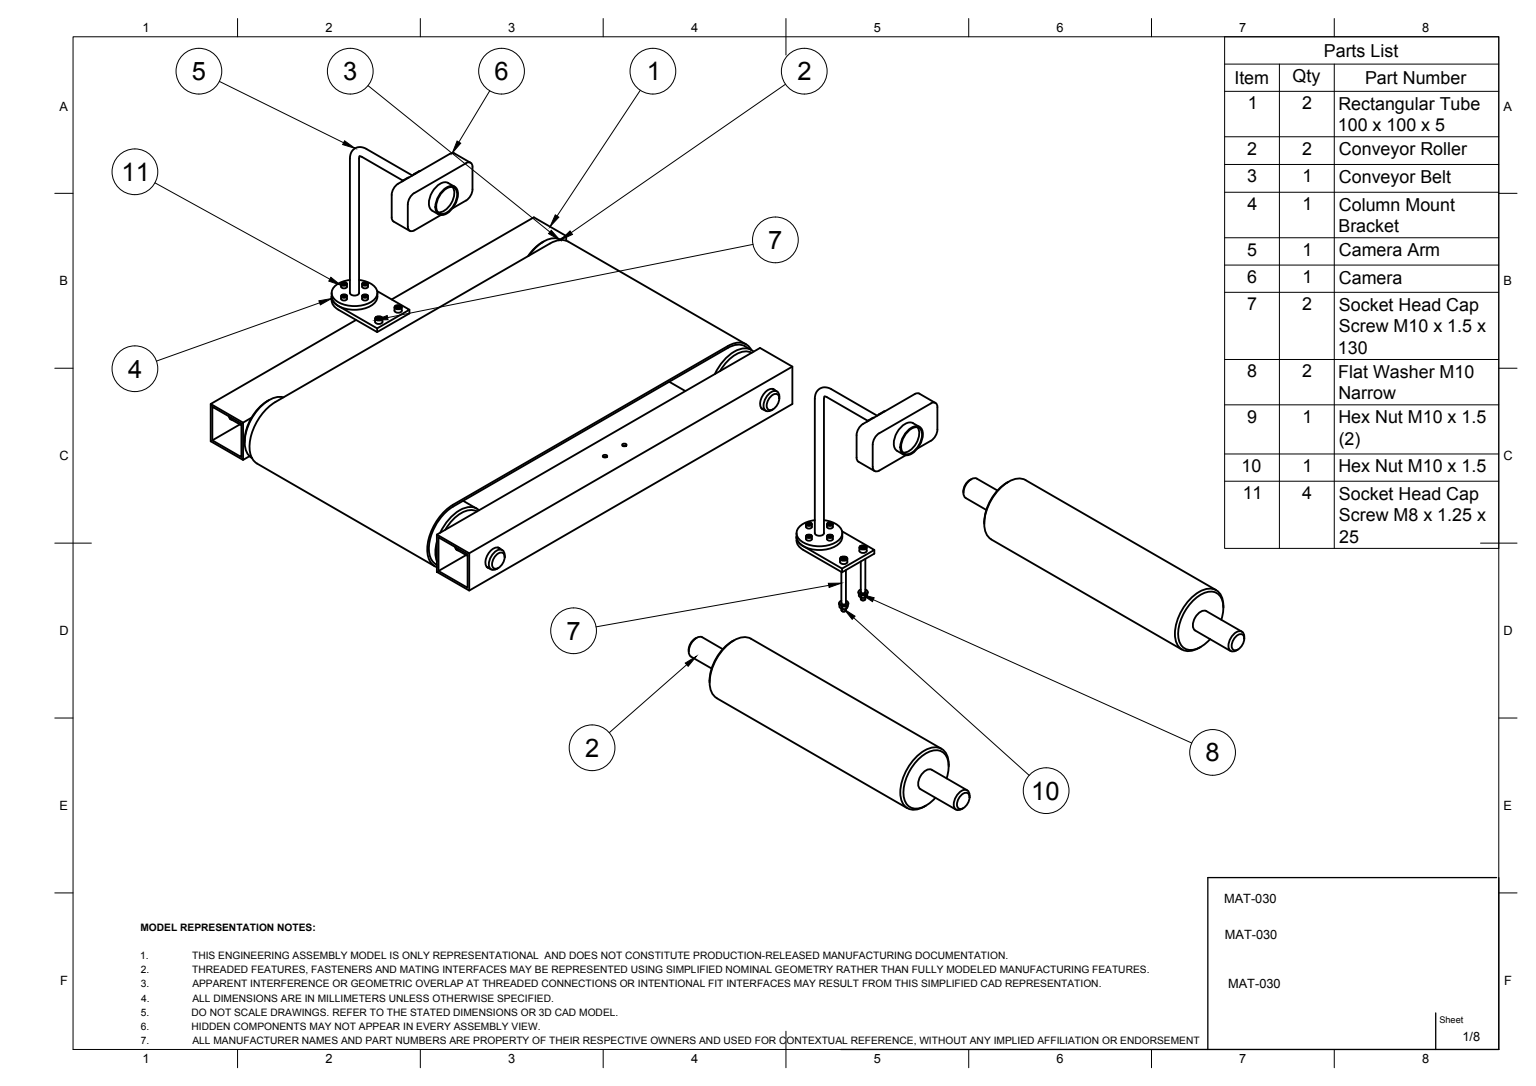
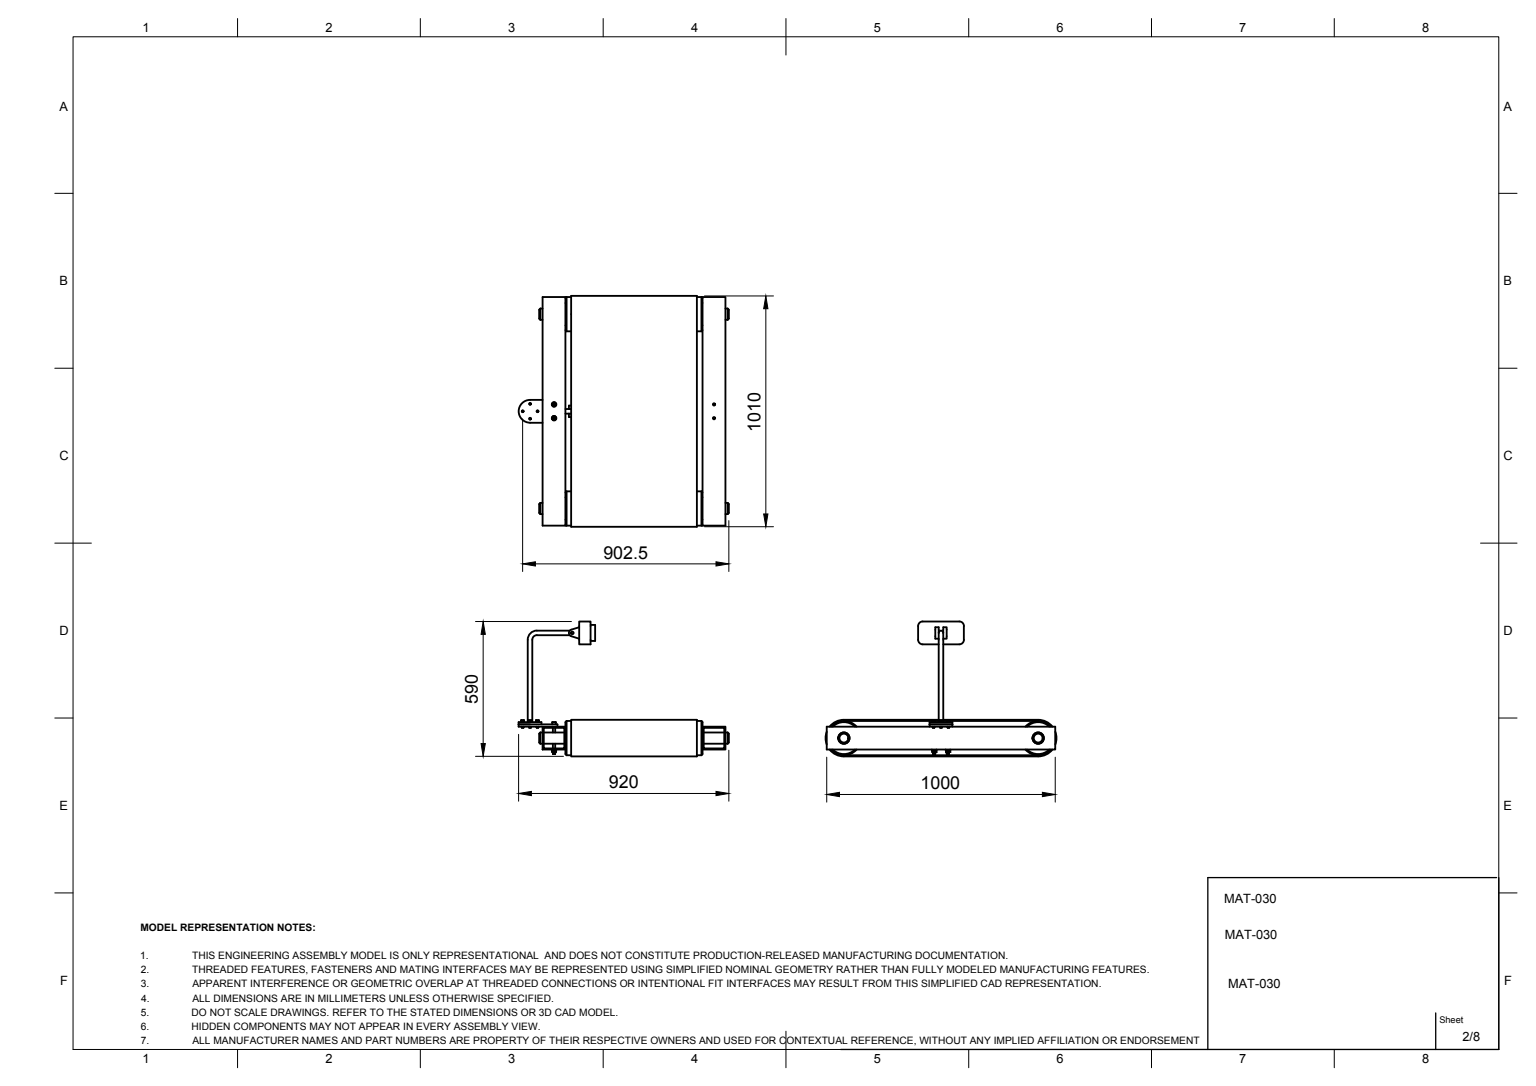
ISO-10303-21;
HEADER;
/* Generated by software containing ST-Developer
 * from STEP Tools, Inc. (www.steptools.com) 
 */

FILE_DESCRIPTION(
/* description */ ('STEP AP214'),
/* implementation_level */ '2;1');

FILE_NAME(
/* name */ 'MAT-030.step',
/* time_stamp */ '2026-11-14T06:43:04-08:00',
/* author */ (''),
/* organization */ (''),
/* preprocessor_version */ 'ST-DEVELOPER v20.2',
/* originating_system */ 'Autodesk Translation Framework v15.17.0.0',
/* authorisation */ '');

FILE_SCHEMA (('AUTOMOTIVE_DESIGN { 1 0 10303 214 3 1 1 }'));
ENDSEC;

DATA;
#10=MECHANICAL_DESIGN_GEOMETRIC_PRESENTATION_REPRESENTATION('',(#198,#199,
#200,#201,#202,#203,#204,#205,#206,#207,#208),#5658);
#11=ITEM_DEFINED_TRANSFORMATION($,$,#3397,#3541);
#12=ITEM_DEFINED_TRANSFORMATION($,$,#3432,#3542);
#13=ITEM_DEFINED_TRANSFORMATION($,$,#3194,#3543);
#14=ITEM_DEFINED_TRANSFORMATION($,$,#3213,#3544);
#15=ITEM_DEFINED_TRANSFORMATION($,$,#3240,#3545);
#16=ITEM_DEFINED_TRANSFORMATION($,$,#3278,#3546);
#17=ITEM_DEFINED_TRANSFORMATION($,$,#3456,#3547);
#18=ITEM_DEFINED_TRANSFORMATION($,$,#3494,#3548);
#19=ITEM_DEFINED_TRANSFORMATION($,$,#3325,#3549);
#20=ITEM_DEFINED_TRANSFORMATION($,$,#3361,#3550);
#21=ITEM_DEFINED_TRANSFORMATION($,$,#3503,#3551);
#22=ITEM_DEFINED_TRANSFORMATION($,$,#3397,#3552);
#23=ITEM_DEFINED_TRANSFORMATION($,$,#3432,#3553);
#24=ITEM_DEFINED_TRANSFORMATION($,$,#3456,#3554);
#25=ITEM_DEFINED_TRANSFORMATION($,$,#3494,#3555);
#26=ITEM_DEFINED_TRANSFORMATION($,$,#3503,#3556);
#27=ITEM_DEFINED_TRANSFORMATION($,$,#3503,#3557);
#28=ITEM_DEFINED_TRANSFORMATION($,$,#3503,#3558);
#29=(
REPRESENTATION_RELATIONSHIP($,$,#5712,#5705)
REPRESENTATION_RELATIONSHIP_WITH_TRANSFORMATION(#11)
SHAPE_REPRESENTATION_RELATIONSHIP()
);
#30=(
REPRESENTATION_RELATIONSHIP($,$,#5713,#5705)
REPRESENTATION_RELATIONSHIP_WITH_TRANSFORMATION(#12)
SHAPE_REPRESENTATION_RELATIONSHIP()
);
#31=(
REPRESENTATION_RELATIONSHIP($,$,#5706,#5705)
REPRESENTATION_RELATIONSHIP_WITH_TRANSFORMATION(#13)
SHAPE_REPRESENTATION_RELATIONSHIP()
);
#32=(
REPRESENTATION_RELATIONSHIP($,$,#5707,#5705)
REPRESENTATION_RELATIONSHIP_WITH_TRANSFORMATION(#14)
SHAPE_REPRESENTATION_RELATIONSHIP()
);
#33=(
REPRESENTATION_RELATIONSHIP($,$,#5708,#5705)
REPRESENTATION_RELATIONSHIP_WITH_TRANSFORMATION(#15)
SHAPE_REPRESENTATION_RELATIONSHIP()
);
#34=(
REPRESENTATION_RELATIONSHIP($,$,#5709,#5705)
REPRESENTATION_RELATIONSHIP_WITH_TRANSFORMATION(#16)
SHAPE_REPRESENTATION_RELATIONSHIP()
);
#35=(
REPRESENTATION_RELATIONSHIP($,$,#5714,#5705)
REPRESENTATION_RELATIONSHIP_WITH_TRANSFORMATION(#17)
SHAPE_REPRESENTATION_RELATIONSHIP()
);
#36=(
REPRESENTATION_RELATIONSHIP($,$,#5715,#5705)
REPRESENTATION_RELATIONSHIP_WITH_TRANSFORMATION(#18)
SHAPE_REPRESENTATION_RELATIONSHIP()
);
#37=(
REPRESENTATION_RELATIONSHIP($,$,#5710,#5705)
REPRESENTATION_RELATIONSHIP_WITH_TRANSFORMATION(#19)
SHAPE_REPRESENTATION_RELATIONSHIP()
);
#38=(
REPRESENTATION_RELATIONSHIP($,$,#5711,#5705)
REPRESENTATION_RELATIONSHIP_WITH_TRANSFORMATION(#20)
SHAPE_REPRESENTATION_RELATIONSHIP()
);
#39=(
REPRESENTATION_RELATIONSHIP($,$,#5716,#5705)
REPRESENTATION_RELATIONSHIP_WITH_TRANSFORMATION(#21)
SHAPE_REPRESENTATION_RELATIONSHIP()
);
#40=(
REPRESENTATION_RELATIONSHIP($,$,#5712,#5705)
REPRESENTATION_RELATIONSHIP_WITH_TRANSFORMATION(#22)
SHAPE_REPRESENTATION_RELATIONSHIP()
);
#41=(
REPRESENTATION_RELATIONSHIP($,$,#5713,#5705)
REPRESENTATION_RELATIONSHIP_WITH_TRANSFORMATION(#23)
SHAPE_REPRESENTATION_RELATIONSHIP()
);
#42=(
REPRESENTATION_RELATIONSHIP($,$,#5714,#5705)
REPRESENTATION_RELATIONSHIP_WITH_TRANSFORMATION(#24)
SHAPE_REPRESENTATION_RELATIONSHIP()
);
#43=(
REPRESENTATION_RELATIONSHIP($,$,#5715,#5705)
REPRESENTATION_RELATIONSHIP_WITH_TRANSFORMATION(#25)
SHAPE_REPRESENTATION_RELATIONSHIP()
);
#44=(
REPRESENTATION_RELATIONSHIP($,$,#5716,#5705)
REPRESENTATION_RELATIONSHIP_WITH_TRANSFORMATION(#26)
SHAPE_REPRESENTATION_RELATIONSHIP()
);
#45=(
REPRESENTATION_RELATIONSHIP($,$,#5716,#5705)
REPRESENTATION_RELATIONSHIP_WITH_TRANSFORMATION(#27)
SHAPE_REPRESENTATION_RELATIONSHIP()
);
#46=(
REPRESENTATION_RELATIONSHIP($,$,#5716,#5705)
REPRESENTATION_RELATIONSHIP_WITH_TRANSFORMATION(#28)
SHAPE_REPRESENTATION_RELATIONSHIP()
);
#47=CONTEXT_DEPENDENT_SHAPE_REPRESENTATION(#29,#5687);
#48=CONTEXT_DEPENDENT_SHAPE_REPRESENTATION(#30,#5688);
#49=CONTEXT_DEPENDENT_SHAPE_REPRESENTATION(#31,#5689);
#50=CONTEXT_DEPENDENT_SHAPE_REPRESENTATION(#32,#5690);
#51=CONTEXT_DEPENDENT_SHAPE_REPRESENTATION(#33,#5691);
#52=CONTEXT_DEPENDENT_SHAPE_REPRESENTATION(#34,#5692);
#53=CONTEXT_DEPENDENT_SHAPE_REPRESENTATION(#35,#5693);
#54=CONTEXT_DEPENDENT_SHAPE_REPRESENTATION(#36,#5694);
#55=CONTEXT_DEPENDENT_SHAPE_REPRESENTATION(#37,#5695);
#56=CONTEXT_DEPENDENT_SHAPE_REPRESENTATION(#38,#5696);
#57=CONTEXT_DEPENDENT_SHAPE_REPRESENTATION(#39,#5697);
#58=CONTEXT_DEPENDENT_SHAPE_REPRESENTATION(#40,#5698);
#59=CONTEXT_DEPENDENT_SHAPE_REPRESENTATION(#41,#5699);
#60=CONTEXT_DEPENDENT_SHAPE_REPRESENTATION(#42,#5700);
#61=CONTEXT_DEPENDENT_SHAPE_REPRESENTATION(#43,#5701);
#62=CONTEXT_DEPENDENT_SHAPE_REPRESENTATION(#44,#5702);
#63=CONTEXT_DEPENDENT_SHAPE_REPRESENTATION(#45,#5703);
#64=CONTEXT_DEPENDENT_SHAPE_REPRESENTATION(#46,#5704);
#65=NEXT_ASSEMBLY_USAGE_OCCURRENCE('Rectangular Tube 100 x 100 x 5:1',
'Rectangular Tube 100 x 100 x 5:1','Rectangular Tube 100 x 100 x 5:1',#5718,
#5725,'Rectangular Tube 100 x 100 x 5:1');
#66=NEXT_ASSEMBLY_USAGE_OCCURRENCE('Conveyor Roller:1',
'Conveyor Roller:1','Conveyor Roller:1',#5718,#5726,'Conveyor Roller:1');
#67=NEXT_ASSEMBLY_USAGE_OCCURRENCE('Conveyor Belt:1','Conveyor Belt:1',
'Conveyor Belt:1',#5718,#5719,'Conveyor Belt:1');
#68=NEXT_ASSEMBLY_USAGE_OCCURRENCE('Column Mount Bracket:1',
'Column Mount Bracket:1','Column Mount Bracket:1',#5718,#5720,
'Column Mount Bracket:1');
#69=NEXT_ASSEMBLY_USAGE_OCCURRENCE('Camera Arm:1','Camera Arm:1',
'Camera Arm:1',#5718,#5721,'Camera Arm:1');
#70=NEXT_ASSEMBLY_USAGE_OCCURRENCE('Camera:1','Camera:1','Camera:1',#5718,
#5722,'Camera:1');
#71=NEXT_ASSEMBLY_USAGE_OCCURRENCE(
'Socket Head Cap Screw M10 x 1.5 x 130:1',
'Socket Head Cap Screw M10 x 1.5 x 130:1',
'Socket Head Cap Screw M10 x 1.5 x 130:1',#5718,#5727,
'Socket Head Cap Screw M10 x 1.5 x 130:1');
#72=NEXT_ASSEMBLY_USAGE_OCCURRENCE('Flat Washer M10 Narrow:1',
'Flat Washer M10 Narrow:1','Flat Washer M10 Narrow:1',#5718,#5728,
'Flat Washer M10 Narrow:1');
#73=NEXT_ASSEMBLY_USAGE_OCCURRENCE('Hex Nut M10 x 1.5 (2):1',
'Hex Nut M10 x 1.5 (2):1','Hex Nut M10 x 1.5 (2):1',#5718,#5723,
'Hex Nut M10 x 1.5 (2):1');
#74=NEXT_ASSEMBLY_USAGE_OCCURRENCE('Hex Nut M10 x 1.5:1',
'Hex Nut M10 x 1.5:1','Hex Nut M10 x 1.5:1',#5718,#5724,
'Hex Nut M10 x 1.5:1');
#75=NEXT_ASSEMBLY_USAGE_OCCURRENCE(
'Socket Head Cap Screw M8 x 1.25 x 25:1',
'Socket Head Cap Screw M8 x 1.25 x 25:1',
'Socket Head Cap Screw M8 x 1.25 x 25:1',#5718,#5729,
'Socket Head Cap Screw M8 x 1.25 x 25:1');
#76=NEXT_ASSEMBLY_USAGE_OCCURRENCE('Rectangular Tube 100 x 100 x 5:2',
'Rectangular Tube 100 x 100 x 5:2','Rectangular Tube 100 x 100 x 5:2',#5718,
#5725,'Rectangular Tube 100 x 100 x 5:2');
#77=NEXT_ASSEMBLY_USAGE_OCCURRENCE('Conveyor Roller:2',
'Conveyor Roller:2','Conveyor Roller:2',#5718,#5726,'Conveyor Roller:2');
#78=NEXT_ASSEMBLY_USAGE_OCCURRENCE(
'Socket Head Cap Screw M10 x 1.5 x 130:2',
'Socket Head Cap Screw M10 x 1.5 x 130:2',
'Socket Head Cap Screw M10 x 1.5 x 130:2',#5718,#5727,
'Socket Head Cap Screw M10 x 1.5 x 130:2');
#79=NEXT_ASSEMBLY_USAGE_OCCURRENCE('Flat Washer M10 Narrow:2',
'Flat Washer M10 Narrow:2','Flat Washer M10 Narrow:2',#5718,#5728,
'Flat Washer M10 Narrow:2');
#80=NEXT_ASSEMBLY_USAGE_OCCURRENCE(
'Socket Head Cap Screw M8 x 1.25 x 25:2',
'Socket Head Cap Screw M8 x 1.25 x 25:2',
'Socket Head Cap Screw M8 x 1.25 x 25:2',#5718,#5729,
'Socket Head Cap Screw M8 x 1.25 x 25:2');
#81=NEXT_ASSEMBLY_USAGE_OCCURRENCE(
'Socket Head Cap Screw M8 x 1.25 x 25:3',
'Socket Head Cap Screw M8 x 1.25 x 25:3',
'Socket Head Cap Screw M8 x 1.25 x 25:3',#5718,#5729,
'Socket Head Cap Screw M8 x 1.25 x 25:3');
#82=NEXT_ASSEMBLY_USAGE_OCCURRENCE(
'Socket Head Cap Screw M8 x 1.25 x 25:4',
'Socket Head Cap Screw M8 x 1.25 x 25:4',
'Socket Head Cap Screw M8 x 1.25 x 25:4',#5718,#5729,
'Socket Head Cap Screw M8 x 1.25 x 25:4');
#83=CONICAL_SURFACE('',#3349,8.,1.0471975511966);
#84=CONICAL_SURFACE('',#3350,8.,1.0471975511966);
#85=CONICAL_SURFACE('',#3351,8.,1.0471975511966);
#86=CONICAL_SURFACE('',#3352,8.,1.0471975511966);
#87=CONICAL_SURFACE('',#3353,8.,1.0471975511966);
#88=CONICAL_SURFACE('',#3354,8.,1.0471975511966);
#89=CONICAL_SURFACE('',#3355,8.,1.0471975511966);
#90=CONICAL_SURFACE('',#3356,8.,1.0471975511966);
#91=CONICAL_SURFACE('',#3357,8.,1.0471975511966);
#92=CONICAL_SURFACE('',#3358,8.,1.0471975511966);
#93=CONICAL_SURFACE('',#3359,8.,1.0471975511966);
#94=CONICAL_SURFACE('',#3360,8.,1.0471975511966);
#95=CONICAL_SURFACE('',#3385,8.,1.0471975511966);
#96=CONICAL_SURFACE('',#3386,8.,1.0471975511966);
#97=CONICAL_SURFACE('',#3387,8.,1.0471975511966);
#98=CONICAL_SURFACE('',#3388,8.,1.0471975511966);
#99=CONICAL_SURFACE('',#3389,8.,1.0471975511966);
#100=CONICAL_SURFACE('',#3390,8.,1.0471975511966);
#101=CONICAL_SURFACE('',#3391,8.,1.0471975511966);
#102=CONICAL_SURFACE('',#3392,8.,1.0471975511966);
#103=CONICAL_SURFACE('',#3393,8.,1.0471975511966);
#104=CONICAL_SURFACE('',#3394,8.,1.0471975511966);
#105=CONICAL_SURFACE('',#3395,8.,1.0471975511966);
#106=CONICAL_SURFACE('',#3396,8.,1.0471975511966);
#107=CONICAL_SURFACE('',#3433,70.0000000000001,0.785398163397444);
#108=CONICAL_SURFACE('',#3437,19.5,0.785398163397451);
#109=CONICAL_SURFACE('',#3441,24.5,0.78539816339745);
#110=CONICAL_SURFACE('',#3444,75.,0.785398163397444);
#111=CONICAL_SURFACE('',#3457,4.0575,1.04719755119659);
#112=CONICAL_SURFACE('',#3469,7.,0.785398163397448);
#113=CONICAL_SURFACE('',#3477,4.172,0.785398163397561);
#114=CONICAL_SURFACE('',#3504,3.0475,1.04719755119659);
#115=CONICAL_SURFACE('',#3516,3.3095,0.785398163397565);
#116=CONICAL_SURFACE('',#3524,5.7,0.785398163397447);
#117=(
BOUNDED_CURVE()
B_SPLINE_CURVE(2,(#4998,#4999,#5000),.UNSPECIFIED.,.F.,.F.)
B_SPLINE_CURVE_WITH_KNOTS((3,3),(1.54292191464265,2.47778215640189),
 .UNSPECIFIED.)
CURVE()
GEOMETRIC_REPRESENTATION_ITEM()
RATIONAL_B_SPLINE_CURVE((1.8727241335928,2.01757984944671,2.01757984944671))
REPRESENTATION_ITEM('')
);
#118=(
BOUNDED_CURVE()
B_SPLINE_CURVE(2,(#5002,#5003,#5004),.UNSPECIFIED.,.F.,.F.)
B_SPLINE_CURVE_WITH_KNOTS((3,3),(2.47778215640189,3.41264239816114),
 .UNSPECIFIED.)
CURVE()
GEOMETRIC_REPRESENTATION_ITEM()
RATIONAL_B_SPLINE_CURVE((2.01757984944671,2.01757984944671,1.8727241335928))
REPRESENTATION_ITEM('')
);
#119=(
BOUNDED_CURVE()
B_SPLINE_CURVE(2,(#5008,#5009,#5010),.UNSPECIFIED.,.F.,.F.)
B_SPLINE_CURVE_WITH_KNOTS((3,3),(-2.47778215640189,-1.54292191464263),
 .UNSPECIFIED.)
CURVE()
GEOMETRIC_REPRESENTATION_ITEM()
RATIONAL_B_SPLINE_CURVE((2.01757984944672,2.01757984944672,1.8727241335928))
REPRESENTATION_ITEM('')
);
#120=(
BOUNDED_CURVE()
B_SPLINE_CURVE(2,(#5011,#5012,#5013),.UNSPECIFIED.,.F.,.F.)
B_SPLINE_CURVE_WITH_KNOTS((3,3),(-3.41264239816113,-2.47778215640189),
 .UNSPECIFIED.)
CURVE()
GEOMETRIC_REPRESENTATION_ITEM()
RATIONAL_B_SPLINE_CURVE((1.8727241335928,2.01757984944671,2.01757984944671))
REPRESENTATION_ITEM('')
);
#121=(
BOUNDED_CURVE()
B_SPLINE_CURVE(2,(#5016,#5017,#5018),.UNSPECIFIED.,.F.,.F.)
B_SPLINE_CURVE_WITH_KNOTS((3,3),(1.54292191464264,2.47778215640189),
 .UNSPECIFIED.)
CURVE()
GEOMETRIC_REPRESENTATION_ITEM()
RATIONAL_B_SPLINE_CURVE((1.8727241335928,2.01757984944672,2.01757984944672))
REPRESENTATION_ITEM('')
);
#122=(
BOUNDED_CURVE()
B_SPLINE_CURVE(2,(#5020,#5021,#5022),.UNSPECIFIED.,.F.,.F.)
B_SPLINE_CURVE_WITH_KNOTS((3,3),(2.47778215640189,3.41264239816113),
 .UNSPECIFIED.)
CURVE()
GEOMETRIC_REPRESENTATION_ITEM()
RATIONAL_B_SPLINE_CURVE((2.01757984944672,2.01757984944672,1.87272413359281))
REPRESENTATION_ITEM('')
);
#123=(
BOUNDED_CURVE()
B_SPLINE_CURVE(2,(#5026,#5027,#5028),.UNSPECIFIED.,.F.,.F.)
B_SPLINE_CURVE_WITH_KNOTS((3,3),(-2.47778215640188,-1.54292191464265),
 .UNSPECIFIED.)
CURVE()
GEOMETRIC_REPRESENTATION_ITEM()
RATIONAL_B_SPLINE_CURVE((2.01757984944672,2.01757984944672,1.87272413359281))
REPRESENTATION_ITEM('')
);
#124=(
BOUNDED_CURVE()
B_SPLINE_CURVE(2,(#5029,#5030,#5031),.UNSPECIFIED.,.F.,.F.)
B_SPLINE_CURVE_WITH_KNOTS((3,3),(-3.41264239816114,-2.47778215640188),
 .UNSPECIFIED.)
CURVE()
GEOMETRIC_REPRESENTATION_ITEM()
RATIONAL_B_SPLINE_CURVE((1.8727241335928,2.01757984944672,2.01757984944672))
REPRESENTATION_ITEM('')
);
#125=(
BOUNDED_CURVE()
B_SPLINE_CURVE(2,(#5035,#5036,#5037),.UNSPECIFIED.,.F.,.F.)
B_SPLINE_CURVE_WITH_KNOTS((3,3),(1.54292191464263,2.47778215640189),
 .UNSPECIFIED.)
CURVE()
GEOMETRIC_REPRESENTATION_ITEM()
RATIONAL_B_SPLINE_CURVE((1.8727241335928,2.01757984944671,2.01757984944671))
REPRESENTATION_ITEM('')
);
#126=(
BOUNDED_CURVE()
B_SPLINE_CURVE(2,(#5041,#5042,#5043),.UNSPECIFIED.,.F.,.F.)
B_SPLINE_CURVE_WITH_KNOTS((3,3),(-3.41264239816114,-2.47778215640189),
 .UNSPECIFIED.)
CURVE()
GEOMETRIC_REPRESENTATION_ITEM()
RATIONAL_B_SPLINE_CURVE((1.8727241335928,2.01757984944671,2.01757984944671))
REPRESENTATION_ITEM('')
);
#127=(
BOUNDED_CURVE()
B_SPLINE_CURVE(2,(#5044,#5045,#5046),.UNSPECIFIED.,.F.,.F.)
B_SPLINE_CURVE_WITH_KNOTS((3,3),(-2.47778215640189,-1.54292191464264),
 .UNSPECIFIED.)
CURVE()
GEOMETRIC_REPRESENTATION_ITEM()
RATIONAL_B_SPLINE_CURVE((2.01757984944671,2.01757984944672,1.8727241335928))
REPRESENTATION_ITEM('')
);
#128=(
BOUNDED_CURVE()
B_SPLINE_CURVE(2,(#5047,#5048,#5049),.UNSPECIFIED.,.F.,.F.)
B_SPLINE_CURVE_WITH_KNOTS((3,3),(2.47778215640189,3.41264239816114),
 .UNSPECIFIED.)
CURVE()
GEOMETRIC_REPRESENTATION_ITEM()
RATIONAL_B_SPLINE_CURVE((2.01757984944671,2.01757984944672,1.8727241335928))
REPRESENTATION_ITEM('')
);
#129=(
BOUNDED_CURVE()
B_SPLINE_CURVE(2,(#5052,#5053,#5054),.UNSPECIFIED.,.F.,.F.)
B_SPLINE_CURVE_WITH_KNOTS((3,3),(1.54292191464265,2.47778215640188),
 .UNSPECIFIED.)
CURVE()
GEOMETRIC_REPRESENTATION_ITEM()
RATIONAL_B_SPLINE_CURVE((1.8727241335928,2.01757984944671,2.01757984944671))
REPRESENTATION_ITEM('')
);
#130=(
BOUNDED_CURVE()
B_SPLINE_CURVE(2,(#5056,#5057,#5058),.UNSPECIFIED.,.F.,.F.)
B_SPLINE_CURVE_WITH_KNOTS((3,3),(2.47778215640188,3.41264239816114),
 .UNSPECIFIED.)
CURVE()
GEOMETRIC_REPRESENTATION_ITEM()
RATIONAL_B_SPLINE_CURVE((2.01757984944671,2.01757984944671,1.87272413359279))
REPRESENTATION_ITEM('')
);
#131=(
BOUNDED_CURVE()
B_SPLINE_CURVE(2,(#5062,#5063,#5064),.UNSPECIFIED.,.F.,.F.)
B_SPLINE_CURVE_WITH_KNOTS((3,3),(-2.47778215640188,-1.54292191464263),
 .UNSPECIFIED.)
CURVE()
GEOMETRIC_REPRESENTATION_ITEM()
RATIONAL_B_SPLINE_CURVE((2.01757984944671,2.01757984944671,1.87272413359279))
REPRESENTATION_ITEM('')
);
#132=(
BOUNDED_CURVE()
B_SPLINE_CURVE(2,(#5065,#5066,#5067),.UNSPECIFIED.,.F.,.F.)
B_SPLINE_CURVE_WITH_KNOTS((3,3),(-3.41264239816112,-2.47778215640188),
 .UNSPECIFIED.)
CURVE()
GEOMETRIC_REPRESENTATION_ITEM()
RATIONAL_B_SPLINE_CURVE((1.8727241335928,2.01757984944671,2.01757984944671))
REPRESENTATION_ITEM('')
);
#133=(
BOUNDED_CURVE()
B_SPLINE_CURVE(2,(#5070,#5071,#5072),.UNSPECIFIED.,.F.,.F.)
B_SPLINE_CURVE_WITH_KNOTS((3,3),(1.54292191464265,2.47778215640188),
 .UNSPECIFIED.)
CURVE()
GEOMETRIC_REPRESENTATION_ITEM()
RATIONAL_B_SPLINE_CURVE((1.8727241335928,2.01757984944671,2.01757984944671))
REPRESENTATION_ITEM('')
);
#134=(
BOUNDED_CURVE()
B_SPLINE_CURVE(2,(#5074,#5075,#5076),.UNSPECIFIED.,.F.,.F.)
B_SPLINE_CURVE_WITH_KNOTS((3,3),(2.47778215640188,3.41264239816112),
 .UNSPECIFIED.)
CURVE()
GEOMETRIC_REPRESENTATION_ITEM()
RATIONAL_B_SPLINE_CURVE((2.01757984944671,2.01757984944671,1.8727241335928))
REPRESENTATION_ITEM('')
);
#135=(
BOUNDED_CURVE()
B_SPLINE_CURVE(2,(#5080,#5081,#5082),.UNSPECIFIED.,.F.,.F.)
B_SPLINE_CURVE_WITH_KNOTS((3,3),(-2.47778215640189,-1.54292191464265),
 .UNSPECIFIED.)
CURVE()
GEOMETRIC_REPRESENTATION_ITEM()
RATIONAL_B_SPLINE_CURVE((2.0175798494467,2.01757984944671,1.8727241335928))
REPRESENTATION_ITEM('')
);
#136=(
BOUNDED_CURVE()
B_SPLINE_CURVE(2,(#5083,#5084,#5085),.UNSPECIFIED.,.F.,.F.)
B_SPLINE_CURVE_WITH_KNOTS((3,3),(-3.41264239816112,-2.47778215640189),
 .UNSPECIFIED.)
CURVE()
GEOMETRIC_REPRESENTATION_ITEM()
RATIONAL_B_SPLINE_CURVE((1.8727241335928,2.0175798494467,2.0175798494467))
REPRESENTATION_ITEM('')
);
#137=(
BOUNDED_CURVE()
B_SPLINE_CURVE(2,(#5088,#5089,#5090),.UNSPECIFIED.,.F.,.F.)
B_SPLINE_CURVE_WITH_KNOTS((3,3),(1.54292191464263,2.47778215640189),
 .UNSPECIFIED.)
CURVE()
GEOMETRIC_REPRESENTATION_ITEM()
RATIONAL_B_SPLINE_CURVE((1.8727241335928,2.01757984944671,2.01757984944671))
REPRESENTATION_ITEM('')
);
#138=(
BOUNDED_CURVE()
B_SPLINE_CURVE(2,(#5091,#5092,#5093),.UNSPECIFIED.,.F.,.F.)
B_SPLINE_CURVE_WITH_KNOTS((3,3),(2.47778215640189,3.41264239816113),
 .UNSPECIFIED.)
CURVE()
GEOMETRIC_REPRESENTATION_ITEM()
RATIONAL_B_SPLINE_CURVE((2.01757984944671,2.01757984944671,1.8727241335928))
REPRESENTATION_ITEM('')
);
#139=(
BOUNDED_CURVE()
B_SPLINE_CURVE(2,(#5095,#5096,#5097),.UNSPECIFIED.,.F.,.F.)
B_SPLINE_CURVE_WITH_KNOTS((3,3),(-2.47778215640189,-1.54292191464264),
 .UNSPECIFIED.)
CURVE()
GEOMETRIC_REPRESENTATION_ITEM()
RATIONAL_B_SPLINE_CURVE((2.01757984944671,2.01757984944672,1.8727241335928))
REPRESENTATION_ITEM('')
);
#140=(
BOUNDED_CURVE()
B_SPLINE_CURVE(2,(#5098,#5099,#5100),.UNSPECIFIED.,.F.,.F.)
B_SPLINE_CURVE_WITH_KNOTS((3,3),(-3.41264239816114,-2.47778215640189),
 .UNSPECIFIED.)
CURVE()
GEOMETRIC_REPRESENTATION_ITEM()
RATIONAL_B_SPLINE_CURVE((1.8727241335928,2.01757984944671,2.01757984944671))
REPRESENTATION_ITEM('')
);
#141=(
BOUNDED_CURVE()
B_SPLINE_CURVE(2,(#5139,#5140,#5141),.UNSPECIFIED.,.F.,.F.)
B_SPLINE_CURVE_WITH_KNOTS((3,3),(1.54292191464265,2.47778215640189),
 .UNSPECIFIED.)
CURVE()
GEOMETRIC_REPRESENTATION_ITEM()
RATIONAL_B_SPLINE_CURVE((1.8727241335928,2.01757984944671,2.01757984944671))
REPRESENTATION_ITEM('')
);
#142=(
BOUNDED_CURVE()
B_SPLINE_CURVE(2,(#5143,#5144,#5145),.UNSPECIFIED.,.F.,.F.)
B_SPLINE_CURVE_WITH_KNOTS((3,3),(2.47778215640189,3.41264239816114),
 .UNSPECIFIED.)
CURVE()
GEOMETRIC_REPRESENTATION_ITEM()
RATIONAL_B_SPLINE_CURVE((2.01757984944671,2.01757984944671,1.8727241335928))
REPRESENTATION_ITEM('')
);
#143=(
BOUNDED_CURVE()
B_SPLINE_CURVE(2,(#5149,#5150,#5151),.UNSPECIFIED.,.F.,.F.)
B_SPLINE_CURVE_WITH_KNOTS((3,3),(-2.47778215640189,-1.54292191464263),
 .UNSPECIFIED.)
CURVE()
GEOMETRIC_REPRESENTATION_ITEM()
RATIONAL_B_SPLINE_CURVE((2.01757984944672,2.01757984944672,1.8727241335928))
REPRESENTATION_ITEM('')
);
#144=(
BOUNDED_CURVE()
B_SPLINE_CURVE(2,(#5152,#5153,#5154),.UNSPECIFIED.,.F.,.F.)
B_SPLINE_CURVE_WITH_KNOTS((3,3),(-3.41264239816113,-2.47778215640189),
 .UNSPECIFIED.)
CURVE()
GEOMETRIC_REPRESENTATION_ITEM()
RATIONAL_B_SPLINE_CURVE((1.8727241335928,2.01757984944671,2.01757984944671))
REPRESENTATION_ITEM('')
);
#145=(
BOUNDED_CURVE()
B_SPLINE_CURVE(2,(#5157,#5158,#5159),.UNSPECIFIED.,.F.,.F.)
B_SPLINE_CURVE_WITH_KNOTS((3,3),(1.54292191464264,2.47778215640189),
 .UNSPECIFIED.)
CURVE()
GEOMETRIC_REPRESENTATION_ITEM()
RATIONAL_B_SPLINE_CURVE((1.8727241335928,2.01757984944672,2.01757984944672))
REPRESENTATION_ITEM('')
);
#146=(
BOUNDED_CURVE()
B_SPLINE_CURVE(2,(#5161,#5162,#5163),.UNSPECIFIED.,.F.,.F.)
B_SPLINE_CURVE_WITH_KNOTS((3,3),(2.47778215640189,3.41264239816113),
 .UNSPECIFIED.)
CURVE()
GEOMETRIC_REPRESENTATION_ITEM()
RATIONAL_B_SPLINE_CURVE((2.01757984944672,2.01757984944672,1.87272413359281))
REPRESENTATION_ITEM('')
);
#147=(
BOUNDED_CURVE()
B_SPLINE_CURVE(2,(#5167,#5168,#5169),.UNSPECIFIED.,.F.,.F.)
B_SPLINE_CURVE_WITH_KNOTS((3,3),(-2.47778215640188,-1.54292191464265),
 .UNSPECIFIED.)
CURVE()
GEOMETRIC_REPRESENTATION_ITEM()
RATIONAL_B_SPLINE_CURVE((2.01757984944672,2.01757984944672,1.87272413359281))
REPRESENTATION_ITEM('')
);
#148=(
BOUNDED_CURVE()
B_SPLINE_CURVE(2,(#5170,#5171,#5172),.UNSPECIFIED.,.F.,.F.)
B_SPLINE_CURVE_WITH_KNOTS((3,3),(-3.41264239816114,-2.47778215640188),
 .UNSPECIFIED.)
CURVE()
GEOMETRIC_REPRESENTATION_ITEM()
RATIONAL_B_SPLINE_CURVE((1.8727241335928,2.01757984944672,2.01757984944672))
REPRESENTATION_ITEM('')
);
#149=(
BOUNDED_CURVE()
B_SPLINE_CURVE(2,(#5176,#5177,#5178),.UNSPECIFIED.,.F.,.F.)
B_SPLINE_CURVE_WITH_KNOTS((3,3),(1.54292191464263,2.47778215640189),
 .UNSPECIFIED.)
CURVE()
GEOMETRIC_REPRESENTATION_ITEM()
RATIONAL_B_SPLINE_CURVE((1.8727241335928,2.01757984944671,2.01757984944671))
REPRESENTATION_ITEM('')
);
#150=(
BOUNDED_CURVE()
B_SPLINE_CURVE(2,(#5182,#5183,#5184),.UNSPECIFIED.,.F.,.F.)
B_SPLINE_CURVE_WITH_KNOTS((3,3),(-3.41264239816114,-2.47778215640189),
 .UNSPECIFIED.)
CURVE()
GEOMETRIC_REPRESENTATION_ITEM()
RATIONAL_B_SPLINE_CURVE((1.8727241335928,2.01757984944671,2.01757984944671))
REPRESENTATION_ITEM('')
);
#151=(
BOUNDED_CURVE()
B_SPLINE_CURVE(2,(#5185,#5186,#5187),.UNSPECIFIED.,.F.,.F.)
B_SPLINE_CURVE_WITH_KNOTS((3,3),(-2.47778215640189,-1.54292191464264),
 .UNSPECIFIED.)
CURVE()
GEOMETRIC_REPRESENTATION_ITEM()
RATIONAL_B_SPLINE_CURVE((2.01757984944671,2.01757984944672,1.8727241335928))
REPRESENTATION_ITEM('')
);
#152=(
BOUNDED_CURVE()
B_SPLINE_CURVE(2,(#5188,#5189,#5190),.UNSPECIFIED.,.F.,.F.)
B_SPLINE_CURVE_WITH_KNOTS((3,3),(2.47778215640189,3.41264239816114),
 .UNSPECIFIED.)
CURVE()
GEOMETRIC_REPRESENTATION_ITEM()
RATIONAL_B_SPLINE_CURVE((2.01757984944671,2.01757984944672,1.8727241335928))
REPRESENTATION_ITEM('')
);
#153=(
BOUNDED_CURVE()
B_SPLINE_CURVE(2,(#5193,#5194,#5195),.UNSPECIFIED.,.F.,.F.)
B_SPLINE_CURVE_WITH_KNOTS((3,3),(1.54292191464265,2.47778215640188),
 .UNSPECIFIED.)
CURVE()
GEOMETRIC_REPRESENTATION_ITEM()
RATIONAL_B_SPLINE_CURVE((1.8727241335928,2.01757984944671,2.01757984944671))
REPRESENTATION_ITEM('')
);
#154=(
BOUNDED_CURVE()
B_SPLINE_CURVE(2,(#5197,#5198,#5199),.UNSPECIFIED.,.F.,.F.)
B_SPLINE_CURVE_WITH_KNOTS((3,3),(2.47778215640188,3.41264239816114),
 .UNSPECIFIED.)
CURVE()
GEOMETRIC_REPRESENTATION_ITEM()
RATIONAL_B_SPLINE_CURVE((2.01757984944671,2.01757984944671,1.87272413359279))
REPRESENTATION_ITEM('')
);
#155=(
BOUNDED_CURVE()
B_SPLINE_CURVE(2,(#5203,#5204,#5205),.UNSPECIFIED.,.F.,.F.)
B_SPLINE_CURVE_WITH_KNOTS((3,3),(-2.47778215640188,-1.54292191464263),
 .UNSPECIFIED.)
CURVE()
GEOMETRIC_REPRESENTATION_ITEM()
RATIONAL_B_SPLINE_CURVE((2.01757984944671,2.01757984944671,1.87272413359279))
REPRESENTATION_ITEM('')
);
#156=(
BOUNDED_CURVE()
B_SPLINE_CURVE(2,(#5206,#5207,#5208),.UNSPECIFIED.,.F.,.F.)
B_SPLINE_CURVE_WITH_KNOTS((3,3),(-3.41264239816112,-2.47778215640188),
 .UNSPECIFIED.)
CURVE()
GEOMETRIC_REPRESENTATION_ITEM()
RATIONAL_B_SPLINE_CURVE((1.8727241335928,2.01757984944671,2.01757984944671))
REPRESENTATION_ITEM('')
);
#157=(
BOUNDED_CURVE()
B_SPLINE_CURVE(2,(#5211,#5212,#5213),.UNSPECIFIED.,.F.,.F.)
B_SPLINE_CURVE_WITH_KNOTS((3,3),(1.54292191464265,2.47778215640188),
 .UNSPECIFIED.)
CURVE()
GEOMETRIC_REPRESENTATION_ITEM()
RATIONAL_B_SPLINE_CURVE((1.8727241335928,2.01757984944671,2.01757984944671))
REPRESENTATION_ITEM('')
);
#158=(
BOUNDED_CURVE()
B_SPLINE_CURVE(2,(#5215,#5216,#5217),.UNSPECIFIED.,.F.,.F.)
B_SPLINE_CURVE_WITH_KNOTS((3,3),(2.47778215640188,3.41264239816112),
 .UNSPECIFIED.)
CURVE()
GEOMETRIC_REPRESENTATION_ITEM()
RATIONAL_B_SPLINE_CURVE((2.01757984944671,2.01757984944671,1.8727241335928))
REPRESENTATION_ITEM('')
);
#159=(
BOUNDED_CURVE()
B_SPLINE_CURVE(2,(#5221,#5222,#5223),.UNSPECIFIED.,.F.,.F.)
B_SPLINE_CURVE_WITH_KNOTS((3,3),(-2.47778215640189,-1.54292191464265),
 .UNSPECIFIED.)
CURVE()
GEOMETRIC_REPRESENTATION_ITEM()
RATIONAL_B_SPLINE_CURVE((2.0175798494467,2.01757984944671,1.8727241335928))
REPRESENTATION_ITEM('')
);
#160=(
BOUNDED_CURVE()
B_SPLINE_CURVE(2,(#5224,#5225,#5226),.UNSPECIFIED.,.F.,.F.)
B_SPLINE_CURVE_WITH_KNOTS((3,3),(-3.41264239816112,-2.47778215640189),
 .UNSPECIFIED.)
CURVE()
GEOMETRIC_REPRESENTATION_ITEM()
RATIONAL_B_SPLINE_CURVE((1.8727241335928,2.0175798494467,2.0175798494467))
REPRESENTATION_ITEM('')
);
#161=(
BOUNDED_CURVE()
B_SPLINE_CURVE(2,(#5229,#5230,#5231),.UNSPECIFIED.,.F.,.F.)
B_SPLINE_CURVE_WITH_KNOTS((3,3),(1.54292191464263,2.47778215640189),
 .UNSPECIFIED.)
CURVE()
GEOMETRIC_REPRESENTATION_ITEM()
RATIONAL_B_SPLINE_CURVE((1.8727241335928,2.01757984944671,2.01757984944671))
REPRESENTATION_ITEM('')
);
#162=(
BOUNDED_CURVE()
B_SPLINE_CURVE(2,(#5232,#5233,#5234),.UNSPECIFIED.,.F.,.F.)
B_SPLINE_CURVE_WITH_KNOTS((3,3),(2.47778215640189,3.41264239816113),
 .UNSPECIFIED.)
CURVE()
GEOMETRIC_REPRESENTATION_ITEM()
RATIONAL_B_SPLINE_CURVE((2.01757984944671,2.01757984944671,1.8727241335928))
REPRESENTATION_ITEM('')
);
#163=(
BOUNDED_CURVE()
B_SPLINE_CURVE(2,(#5236,#5237,#5238),.UNSPECIFIED.,.F.,.F.)
B_SPLINE_CURVE_WITH_KNOTS((3,3),(-2.47778215640189,-1.54292191464264),
 .UNSPECIFIED.)
CURVE()
GEOMETRIC_REPRESENTATION_ITEM()
RATIONAL_B_SPLINE_CURVE((2.01757984944671,2.01757984944672,1.8727241335928))
REPRESENTATION_ITEM('')
);
#164=(
BOUNDED_CURVE()
B_SPLINE_CURVE(2,(#5239,#5240,#5241),.UNSPECIFIED.,.F.,.F.)
B_SPLINE_CURVE_WITH_KNOTS((3,3),(-3.41264239816114,-2.47778215640189),
 .UNSPECIFIED.)
CURVE()
GEOMETRIC_REPRESENTATION_ITEM()
RATIONAL_B_SPLINE_CURVE((1.8727241335928,2.01757984944671,2.01757984944671))
REPRESENTATION_ITEM('')
);
#165=(
BOUNDED_SURFACE()
B_SPLINE_SURFACE(2,2,((#4850,#4851,#4852,#4853,#4854,#4855,#4856,#4857,
#4858),(#4859,#4860,#4861,#4862,#4863,#4864,#4865,#4866,#4867),(#4868,#4869,
#4870,#4871,#4872,#4873,#4874,#4875,#4876)),.UNSPECIFIED.,.F.,.T.,.F.)
B_SPLINE_SURFACE_WITH_KNOTS((3,3),(3,2,2,2,3),(-1.55552293509789,-1.0706447979528),
(-3.14159265358979,-1.5707963267949,0.,1.5707963267949,3.14159265358979),
 .UNSPECIFIED.)
GEOMETRIC_REPRESENTATION_ITEM()
RATIONAL_B_SPLINE_SURFACE(((1.,0.707106781186548,1.,0.707106781186548,1.,
0.707106781186548,1.,0.707106781186548,1.),(0.970755313150814,0.686427664801811,
0.970755313150814,0.686427664801811,0.970755313150814,0.686427664801811,
0.970755313150814,0.686427664801811,0.970755313150814),(1.,0.707106781186548,
1.,0.707106781186548,1.,0.707106781186548,1.,0.707106781186548,1.)))
REPRESENTATION_ITEM('')
SURFACE()
);
#166=B_SPLINE_CURVE_WITH_KNOTS('',3,(#4617,#4618,#4619,#4620,#4621,#4622,
#4623,#4624,#4625,#4626,#4627,#4628,#4629,#4630,#4631,#4632,#4633,#4634,
#4635,#4636,#4637,#4638,#4639,#4640,#4641,#4642,#4643,#4644,#4645,#4646,
#4647,#4648,#4649,#4650),.UNSPECIFIED.,.T.,.F.,(4,2,2,2,2,2,2,2,2,2,2,2,
2,2,2,2,4),(0.,0.212929378403861,0.425858756807722,0.637884496210834,0.849910235613946,
1.06193597501706,1.27396171442017,1.48689109282403,1.69982047122789,1.91274984963175,
2.12567922803561,2.33770496743873,2.54973070684184,2.76175644624495,2.97378218564806,
3.18671156405192,3.39964094245578),.UNSPECIFIED.);
#167=B_SPLINE_CURVE_WITH_KNOTS('',3,(#4654,#4655,#4656,#4657,#4658,#4659,
#4660,#4661,#4662,#4663,#4664,#4665,#4666,#4667,#4668,#4669,#4670,#4671,
#4672,#4673,#4674,#4675),.UNSPECIFIED.,.F.,.F.,(4,2,2,2,2,2,2,2,2,2,4),
(-1.76955541861604,-1.65739985744517,-1.5452442962743,-1.32093317393256,
-1.10285544162029,-0.884777709308018,-0.666699976995746,-0.448622244683475,
-0.224311122341738,-0.112155561170869,0.),.UNSPECIFIED.);
#168=B_SPLINE_CURVE_WITH_KNOTS('',3,(#4676,#4677,#4678,#4679,#4680,#4681,
#4682,#4683,#4684,#4685,#4686,#4687,#4688,#4689,#4690,#4691,#4692,#4693,
#4694,#4695,#4696,#4697),.UNSPECIFIED.,.F.,.F.,(4,2,2,2,2,2,2,2,2,2,4),
(-3.53911083723207,-3.4269552760612,-3.31479971489033,-3.0904885925486,
-2.87241086023632,-2.65433312792405,-2.43625539561178,-2.21817766329951,
-1.99386654095777,-1.8817109797869,-1.76955541861604),.UNSPECIFIED.);
#169=B_SPLINE_CURVE_WITH_KNOTS('',3,(#4701,#4702,#4703,#4704,#4705,#4706,
#4707,#4708,#4709,#4710,#4711,#4712,#4713,#4714,#4715,#4716,#4717,#4718,
#4719,#4720,#4721,#4722),.UNSPECIFIED.,.F.,.F.,(4,2,2,2,2,2,2,2,2,2,4),
(0.,0.112155561170869,0.224311122341738,0.448622244683475,0.666699976995746,
0.884777709308018,1.10285544162029,1.32093317393256,1.5452442962743,1.65739985744517,
1.76955541861604),.UNSPECIFIED.);
#170=B_SPLINE_CURVE_WITH_KNOTS('',3,(#4725,#4726,#4727,#4728,#4729,#4730,
#4731,#4732,#4733,#4734,#4735,#4736,#4737,#4738,#4739,#4740,#4741,#4742,
#4743,#4744,#4745,#4746,#4747,#4748,#4749,#4750,#4751,#4752,#4753,#4754,
#4755,#4756,#4757,#4758),.UNSPECIFIED.,.T.,.F.,(4,2,2,2,2,2,2,2,2,2,2,2,
2,2,2,2,4),(-3.39964094245578,-3.18671156405192,-2.97378218564806,-2.76175644624495,
-2.54973070684184,-2.33770496743873,-2.12567922803561,-1.91274984963175,
-1.69982047122789,-1.48689109282403,-1.27396171442017,-1.06193597501706,
-0.849910235613946,-0.637884496210834,-0.425858756807722,-0.212929378403861,
0.),.UNSPECIFIED.);
#171=B_SPLINE_CURVE_WITH_KNOTS('',3,(#4759,#4760,#4761,#4762,#4763,#4764,
#4765,#4766,#4767,#4768,#4769,#4770,#4771,#4772,#4773,#4774,#4775,#4776,
#4777,#4778,#4779,#4780),.UNSPECIFIED.,.F.,.F.,(4,2,2,2,2,2,2,2,2,2,4),
(1.76955541861604,1.8817109797869,1.99386654095777,2.21817766329951,2.43625539561178,
2.65433312792405,2.87241086023632,3.0904885925486,3.31479971489033,3.4269552760612,
3.53911083723207),.UNSPECIFIED.);
#172=TOROIDAL_SURFACE('',#3241,30.,7.);
#173=TOROIDAL_SURFACE('',#3245,30.,10.);
#174=TOROIDAL_SURFACE('',#3464,5.40000000000003,0.4);
#175=TOROIDAL_SURFACE('',#3511,4.40000000000003,0.4);
#176=SHAPE_REPRESENTATION_RELATIONSHIP('SRR','None',#5706,#187);
#177=SHAPE_REPRESENTATION_RELATIONSHIP('SRR','None',#5707,#188);
#178=SHAPE_REPRESENTATION_RELATIONSHIP('SRR','None',#5708,#189);
#179=SHAPE_REPRESENTATION_RELATIONSHIP('SRR','None',#5709,#190);
#180=SHAPE_REPRESENTATION_RELATIONSHIP('SRR','None',#5710,#191);
#181=SHAPE_REPRESENTATION_RELATIONSHIP('SRR','None',#5711,#192);
#182=SHAPE_REPRESENTATION_RELATIONSHIP('SRR','None',#5712,#193);
#183=SHAPE_REPRESENTATION_RELATIONSHIP('SRR','None',#5713,#194);
#184=SHAPE_REPRESENTATION_RELATIONSHIP('SRR','None',#5714,#195);
#185=SHAPE_REPRESENTATION_RELATIONSHIP('SRR','None',#5715,#196);
#186=SHAPE_REPRESENTATION_RELATIONSHIP('SRR','None',#5716,#197);
#187=ADVANCED_BREP_SHAPE_REPRESENTATION('',(#209),#5647);
#188=ADVANCED_BREP_SHAPE_REPRESENTATION('',(#210),#5648);
#189=ADVANCED_BREP_SHAPE_REPRESENTATION('',(#211),#5649);
#190=ADVANCED_BREP_SHAPE_REPRESENTATION('',(#212),#5650);
#191=ADVANCED_BREP_SHAPE_REPRESENTATION('',(#213),#5651);
#192=ADVANCED_BREP_SHAPE_REPRESENTATION('',(#214),#5652);
#193=ADVANCED_BREP_SHAPE_REPRESENTATION('',(#215),#5653);
#194=ADVANCED_BREP_SHAPE_REPRESENTATION('',(#216),#5654);
#195=ADVANCED_BREP_SHAPE_REPRESENTATION('',(#217),#5655);
#196=ADVANCED_BREP_SHAPE_REPRESENTATION('',(#218),#5656);
#197=ADVANCED_BREP_SHAPE_REPRESENTATION('',(#219),#5657);
#198=STYLED_ITEM('',(#5770),#209);
#199=STYLED_ITEM('',(#5771),#210);
#200=STYLED_ITEM('',(#5772),#211);
#201=STYLED_ITEM('',(#5772),#212);
#202=STYLED_ITEM('',(#5770),#213);
#203=STYLED_ITEM('',(#5770),#214);
#204=STYLED_ITEM('',(#5772),#215);
#205=STYLED_ITEM('',(#5773),#216);
#206=STYLED_ITEM('',(#5770),#217);
#207=STYLED_ITEM('',(#5770),#218);
#208=STYLED_ITEM('',(#5770),#219);
#209=MANIFOLD_SOLID_BREP('Body1',#3060);
#210=MANIFOLD_SOLID_BREP('Body1',#3061);
#211=MANIFOLD_SOLID_BREP('Body1',#3062);
#212=MANIFOLD_SOLID_BREP('Body1',#3063);
#213=MANIFOLD_SOLID_BREP('Body1',#3064);
#214=MANIFOLD_SOLID_BREP('Body1',#3065);
#215=MANIFOLD_SOLID_BREP('Body1',#3066);
#216=MANIFOLD_SOLID_BREP('Body1',#3067);
#217=MANIFOLD_SOLID_BREP('Body1',#3068);
#218=MANIFOLD_SOLID_BREP('Body1',#3069);
#219=MANIFOLD_SOLID_BREP('Body1',#3070);
#220=CYLINDRICAL_SURFACE('',#3205,80.);
#221=CYLINDRICAL_SURFACE('',#3207,80.);
#222=CYLINDRICAL_SURFACE('',#3209,75.);
#223=CYLINDRICAL_SURFACE('',#3211,75.);
#224=CYLINDRICAL_SURFACE('',#3214,4.);
#225=CYLINDRICAL_SURFACE('',#3217,4.);
#226=CYLINDRICAL_SURFACE('',#3220,4.);
#227=CYLINDRICAL_SURFACE('',#3223,3.99999999999999);
#228=CYLINDRICAL_SURFACE('',#3226,5.75);
#229=CYLINDRICAL_SURFACE('',#3229,5.75000000000001);
#230=CYLINDRICAL_SURFACE('',#3238,50.0000000000001);
#231=CYLINDRICAL_SURFACE('',#3249,5.50000000000001);
#232=CYLINDRICAL_SURFACE('',#3250,5.50000000000001);
#233=CYLINDRICAL_SURFACE('',#3251,4.);
#234=CYLINDRICAL_SURFACE('',#3254,4.);
#235=CYLINDRICAL_SURFACE('',#3257,4.);
#236=CYLINDRICAL_SURFACE('',#3260,4.00000000000001);
#237=CYLINDRICAL_SURFACE('',#3263,50.);
#238=CYLINDRICAL_SURFACE('',#3266,7.);
#239=CYLINDRICAL_SURFACE('',#3268,7.00000000000001);
#240=CYLINDRICAL_SURFACE('',#3270,10.);
#241=CYLINDRICAL_SURFACE('',#3272,10.);
#242=CYLINDRICAL_SURFACE('',#3279,5.5);
#243=CYLINDRICAL_SURFACE('',#3282,5.5);
#244=CYLINDRICAL_SURFACE('',#3285,35.);
#245=CYLINDRICAL_SURFACE('',#3290,32.5);
#246=CYLINDRICAL_SURFACE('',#3292,15.);
#247=CYLINDRICAL_SURFACE('',#3297,20.);
#248=CYLINDRICAL_SURFACE('',#3301,20.);
#249=CYLINDRICAL_SURFACE('',#3305,20.);
#250=CYLINDRICAL_SURFACE('',#3309,20.);
#251=CYLINDRICAL_SURFACE('',#3316,15.);
#252=CYLINDRICAL_SURFACE('',#3326,5.);
#253=CYLINDRICAL_SURFACE('',#3362,5.);
#254=CYLINDRICAL_SURFACE('',#3398,5.);
#255=CYLINDRICAL_SURFACE('',#3401,5.);
#256=CYLINDRICAL_SURFACE('',#3404,5.);
#257=CYLINDRICAL_SURFACE('',#3407,5.);
#258=CYLINDRICAL_SURFACE('',#3410,25.);
#259=CYLINDRICAL_SURFACE('',#3413,25.);
#260=CYLINDRICAL_SURFACE('',#3416,25.);
#261=CYLINDRICAL_SURFACE('',#3419,25.);
#262=CYLINDRICAL_SURFACE('',#3447,75.);
#263=CYLINDRICAL_SURFACE('',#3448,24.5);
#264=CYLINDRICAL_SURFACE('',#3450,24.5);
#265=CYLINDRICAL_SURFACE('',#3473,8.);
#266=CYLINDRICAL_SURFACE('',#3475,5.00000000000003);
#267=CYLINDRICAL_SURFACE('',#3495,10.);
#268=CYLINDRICAL_SURFACE('',#3498,5.56);
#269=CYLINDRICAL_SURFACE('',#3519,4.00000000000003);
#270=CYLINDRICAL_SURFACE('',#3520,6.5);
#271=FACE_BOUND('',#520,.T.);
#272=FACE_BOUND('',#522,.T.);
#273=FACE_BOUND('',#538,.T.);
#274=FACE_BOUND('',#539,.T.);
#275=FACE_BOUND('',#540,.T.);
#276=FACE_BOUND('',#541,.T.);
#277=FACE_BOUND('',#542,.T.);
#278=FACE_BOUND('',#543,.T.);
#279=FACE_BOUND('',#545,.T.);
#280=FACE_BOUND('',#546,.T.);
#281=FACE_BOUND('',#547,.T.);
#282=FACE_BOUND('',#548,.T.);
#283=FACE_BOUND('',#549,.T.);
#284=FACE_BOUND('',#550,.T.);
#285=FACE_BOUND('',#566,.T.);
#286=FACE_BOUND('',#567,.T.);
#287=FACE_BOUND('',#570,.T.);
#288=FACE_BOUND('',#571,.T.);
#289=FACE_BOUND('',#573,.T.);
#290=FACE_BOUND('',#576,.T.);
#291=FACE_BOUND('',#577,.T.);
#292=FACE_BOUND('',#578,.T.);
#293=FACE_BOUND('',#579,.T.);
#294=FACE_BOUND('',#580,.T.);
#295=FACE_BOUND('',#582,.T.);
#296=FACE_BOUND('',#583,.T.);
#297=FACE_BOUND('',#584,.T.);
#298=FACE_BOUND('',#585,.T.);
#299=FACE_BOUND('',#603,.T.);
#300=FACE_BOUND('',#604,.T.);
#301=FACE_BOUND('',#606,.T.);
#302=FACE_BOUND('',#608,.T.);
#303=FACE_BOUND('',#613,.T.);
#304=FACE_BOUND('',#615,.T.);
#305=FACE_BOUND('',#617,.T.);
#306=FACE_BOUND('',#619,.T.);
#307=FACE_BOUND('',#628,.T.);
#308=FACE_BOUND('',#630,.T.);
#309=FACE_BOUND('',#651,.T.);
#310=FACE_BOUND('',#653,.T.);
#311=FACE_BOUND('',#675,.T.);
#312=FACE_BOUND('',#677,.T.);
#313=FACE_BOUND('',#679,.T.);
#314=FACE_BOUND('',#680,.T.);
#315=FACE_BOUND('',#682,.T.);
#316=FACE_BOUND('',#683,.T.);
#317=FACE_BOUND('',#685,.T.);
#318=FACE_BOUND('',#686,.T.);
#319=FACE_BOUND('',#688,.T.);
#320=FACE_BOUND('',#689,.T.);
#321=FACE_BOUND('',#691,.T.);
#322=FACE_BOUND('',#692,.T.);
#323=FACE_BOUND('',#694,.T.);
#324=FACE_BOUND('',#695,.T.);
#325=FACE_BOUND('',#697,.T.);
#326=FACE_BOUND('',#698,.T.);
#327=FACE_BOUND('',#700,.T.);
#328=FACE_BOUND('',#701,.T.);
#329=FACE_BOUND('',#711,.T.);
#330=FACE_BOUND('',#713,.T.);
#331=FACE_BOUND('',#722,.T.);
#332=FACE_BOUND('',#725,.T.);
#333=FACE_BOUND('',#741,.T.);
#334=FACE_BOUND('',#743,.T.);
#335=FACE_BOUND('',#751,.T.);
#336=FACE_BOUND('',#753,.T.);
#337=FACE_OUTER_BOUND('',#519,.T.);
#338=FACE_OUTER_BOUND('',#521,.T.);
#339=FACE_OUTER_BOUND('',#523,.T.);
#340=FACE_OUTER_BOUND('',#524,.T.);
#341=FACE_OUTER_BOUND('',#525,.T.);
#342=FACE_OUTER_BOUND('',#526,.T.);
#343=FACE_OUTER_BOUND('',#527,.T.);
#344=FACE_OUTER_BOUND('',#528,.T.);
#345=FACE_OUTER_BOUND('',#529,.T.);
#346=FACE_OUTER_BOUND('',#530,.T.);
#347=FACE_OUTER_BOUND('',#531,.T.);
#348=FACE_OUTER_BOUND('',#532,.T.);
#349=FACE_OUTER_BOUND('',#533,.T.);
#350=FACE_OUTER_BOUND('',#534,.T.);
#351=FACE_OUTER_BOUND('',#535,.T.);
#352=FACE_OUTER_BOUND('',#536,.T.);
#353=FACE_OUTER_BOUND('',#537,.T.);
#354=FACE_OUTER_BOUND('',#544,.T.);
#355=FACE_OUTER_BOUND('',#551,.T.);
#356=FACE_OUTER_BOUND('',#552,.T.);
#357=FACE_OUTER_BOUND('',#553,.T.);
#358=FACE_OUTER_BOUND('',#554,.T.);
#359=FACE_OUTER_BOUND('',#555,.T.);
#360=FACE_OUTER_BOUND('',#556,.T.);
#361=FACE_OUTER_BOUND('',#557,.T.);
#362=FACE_OUTER_BOUND('',#558,.T.);
#363=FACE_OUTER_BOUND('',#559,.T.);
#364=FACE_OUTER_BOUND('',#560,.T.);
#365=FACE_OUTER_BOUND('',#561,.T.);
#366=FACE_OUTER_BOUND('',#562,.T.);
#367=FACE_OUTER_BOUND('',#563,.T.);
#368=FACE_OUTER_BOUND('',#564,.T.);
#369=FACE_OUTER_BOUND('',#565,.T.);
#370=FACE_OUTER_BOUND('',#568,.T.);
#371=FACE_OUTER_BOUND('',#569,.T.);
#372=FACE_OUTER_BOUND('',#572,.T.);
#373=FACE_OUTER_BOUND('',#574,.T.);
#374=FACE_OUTER_BOUND('',#575,.T.);
#375=FACE_OUTER_BOUND('',#581,.T.);
#376=FACE_OUTER_BOUND('',#586,.T.);
#377=FACE_OUTER_BOUND('',#587,.T.);
#378=FACE_OUTER_BOUND('',#588,.T.);
#379=FACE_OUTER_BOUND('',#589,.T.);
#380=FACE_OUTER_BOUND('',#590,.T.);
#381=FACE_OUTER_BOUND('',#591,.T.);
#382=FACE_OUTER_BOUND('',#592,.T.);
#383=FACE_OUTER_BOUND('',#593,.T.);
#384=FACE_OUTER_BOUND('',#594,.T.);
#385=FACE_OUTER_BOUND('',#595,.T.);
#386=FACE_OUTER_BOUND('',#596,.T.);
#387=FACE_OUTER_BOUND('',#597,.T.);
#388=FACE_OUTER_BOUND('',#598,.T.);
#389=FACE_OUTER_BOUND('',#599,.T.);
#390=FACE_OUTER_BOUND('',#600,.T.);
#391=FACE_OUTER_BOUND('',#601,.T.);
#392=FACE_OUTER_BOUND('',#602,.T.);
#393=FACE_OUTER_BOUND('',#605,.T.);
#394=FACE_OUTER_BOUND('',#607,.T.);
#395=FACE_OUTER_BOUND('',#609,.T.);
#396=FACE_OUTER_BOUND('',#610,.T.);
#397=FACE_OUTER_BOUND('',#611,.T.);
#398=FACE_OUTER_BOUND('',#612,.T.);
#399=FACE_OUTER_BOUND('',#614,.T.);
#400=FACE_OUTER_BOUND('',#616,.T.);
#401=FACE_OUTER_BOUND('',#618,.T.);
#402=FACE_OUTER_BOUND('',#620,.T.);
#403=FACE_OUTER_BOUND('',#621,.T.);
#404=FACE_OUTER_BOUND('',#622,.T.);
#405=FACE_OUTER_BOUND('',#623,.T.);
#406=FACE_OUTER_BOUND('',#624,.T.);
#407=FACE_OUTER_BOUND('',#625,.T.);
#408=FACE_OUTER_BOUND('',#626,.T.);
#409=FACE_OUTER_BOUND('',#627,.T.);
#410=FACE_OUTER_BOUND('',#629,.T.);
#411=FACE_OUTER_BOUND('',#631,.T.);
#412=FACE_OUTER_BOUND('',#632,.T.);
#413=FACE_OUTER_BOUND('',#633,.T.);
#414=FACE_OUTER_BOUND('',#634,.T.);
#415=FACE_OUTER_BOUND('',#635,.T.);
#416=FACE_OUTER_BOUND('',#636,.T.);
#417=FACE_OUTER_BOUND('',#637,.T.);
#418=FACE_OUTER_BOUND('',#638,.T.);
#419=FACE_OUTER_BOUND('',#639,.T.);
#420=FACE_OUTER_BOUND('',#640,.T.);
#421=FACE_OUTER_BOUND('',#641,.T.);
#422=FACE_OUTER_BOUND('',#642,.T.);
#423=FACE_OUTER_BOUND('',#643,.T.);
#424=FACE_OUTER_BOUND('',#644,.T.);
#425=FACE_OUTER_BOUND('',#645,.T.);
#426=FACE_OUTER_BOUND('',#646,.T.);
#427=FACE_OUTER_BOUND('',#647,.T.);
#428=FACE_OUTER_BOUND('',#648,.T.);
#429=FACE_OUTER_BOUND('',#649,.T.);
#430=FACE_OUTER_BOUND('',#650,.T.);
#431=FACE_OUTER_BOUND('',#652,.T.);
#432=FACE_OUTER_BOUND('',#654,.T.);
#433=FACE_OUTER_BOUND('',#655,.T.);
#434=FACE_OUTER_BOUND('',#656,.T.);
#435=FACE_OUTER_BOUND('',#657,.T.);
#436=FACE_OUTER_BOUND('',#658,.T.);
#437=FACE_OUTER_BOUND('',#659,.T.);
#438=FACE_OUTER_BOUND('',#660,.T.);
#439=FACE_OUTER_BOUND('',#661,.T.);
#440=FACE_OUTER_BOUND('',#662,.T.);
#441=FACE_OUTER_BOUND('',#663,.T.);
#442=FACE_OUTER_BOUND('',#664,.T.);
#443=FACE_OUTER_BOUND('',#665,.T.);
#444=FACE_OUTER_BOUND('',#666,.T.);
#445=FACE_OUTER_BOUND('',#667,.T.);
#446=FACE_OUTER_BOUND('',#668,.T.);
#447=FACE_OUTER_BOUND('',#669,.T.);
#448=FACE_OUTER_BOUND('',#670,.T.);
#449=FACE_OUTER_BOUND('',#671,.T.);
#450=FACE_OUTER_BOUND('',#672,.T.);
#451=FACE_OUTER_BOUND('',#673,.T.);
#452=FACE_OUTER_BOUND('',#674,.T.);
#453=FACE_OUTER_BOUND('',#676,.T.);
#454=FACE_OUTER_BOUND('',#678,.T.);
#455=FACE_OUTER_BOUND('',#681,.T.);
#456=FACE_OUTER_BOUND('',#684,.T.);
#457=FACE_OUTER_BOUND('',#687,.T.);
#458=FACE_OUTER_BOUND('',#690,.T.);
#459=FACE_OUTER_BOUND('',#693,.T.);
#460=FACE_OUTER_BOUND('',#696,.T.);
#461=FACE_OUTER_BOUND('',#699,.T.);
#462=FACE_OUTER_BOUND('',#702,.T.);
#463=FACE_OUTER_BOUND('',#703,.T.);
#464=FACE_OUTER_BOUND('',#704,.T.);
#465=FACE_OUTER_BOUND('',#705,.T.);
#466=FACE_OUTER_BOUND('',#706,.T.);
#467=FACE_OUTER_BOUND('',#707,.T.);
#468=FACE_OUTER_BOUND('',#708,.T.);
#469=FACE_OUTER_BOUND('',#709,.T.);
#470=FACE_OUTER_BOUND('',#710,.T.);
#471=FACE_OUTER_BOUND('',#712,.T.);
#472=FACE_OUTER_BOUND('',#714,.T.);
#473=FACE_OUTER_BOUND('',#715,.T.);
#474=FACE_OUTER_BOUND('',#716,.T.);
#475=FACE_OUTER_BOUND('',#717,.T.);
#476=FACE_OUTER_BOUND('',#718,.T.);
#477=FACE_OUTER_BOUND('',#719,.T.);
#478=FACE_OUTER_BOUND('',#720,.T.);
#479=FACE_OUTER_BOUND('',#721,.T.);
#480=FACE_OUTER_BOUND('',#723,.T.);
#481=FACE_OUTER_BOUND('',#724,.T.);
#482=FACE_OUTER_BOUND('',#726,.T.);
#483=FACE_OUTER_BOUND('',#727,.T.);
#484=FACE_OUTER_BOUND('',#728,.T.);
#485=FACE_OUTER_BOUND('',#729,.T.);
#486=FACE_OUTER_BOUND('',#730,.T.);
#487=FACE_OUTER_BOUND('',#731,.T.);
#488=FACE_OUTER_BOUND('',#732,.T.);
#489=FACE_OUTER_BOUND('',#733,.T.);
#490=FACE_OUTER_BOUND('',#734,.T.);
#491=FACE_OUTER_BOUND('',#735,.T.);
#492=FACE_OUTER_BOUND('',#736,.T.);
#493=FACE_OUTER_BOUND('',#737,.T.);
#494=FACE_OUTER_BOUND('',#738,.T.);
#495=FACE_OUTER_BOUND('',#739,.T.);
#496=FACE_OUTER_BOUND('',#740,.T.);
#497=FACE_OUTER_BOUND('',#742,.T.);
#498=FACE_OUTER_BOUND('',#744,.T.);
#499=FACE_OUTER_BOUND('',#745,.T.);
#500=FACE_OUTER_BOUND('',#746,.T.);
#501=FACE_OUTER_BOUND('',#747,.T.);
#502=FACE_OUTER_BOUND('',#748,.T.);
#503=FACE_OUTER_BOUND('',#749,.T.);
#504=FACE_OUTER_BOUND('',#750,.T.);
#505=FACE_OUTER_BOUND('',#752,.T.);
#506=FACE_OUTER_BOUND('',#754,.T.);
#507=FACE_OUTER_BOUND('',#755,.T.);
#508=FACE_OUTER_BOUND('',#756,.T.);
#509=FACE_OUTER_BOUND('',#757,.T.);
#510=FACE_OUTER_BOUND('',#758,.T.);
#511=FACE_OUTER_BOUND('',#759,.T.);
#512=FACE_OUTER_BOUND('',#760,.T.);
#513=FACE_OUTER_BOUND('',#761,.T.);
#514=FACE_OUTER_BOUND('',#762,.T.);
#515=FACE_OUTER_BOUND('',#763,.T.);
#516=FACE_OUTER_BOUND('',#764,.T.);
#517=FACE_OUTER_BOUND('',#765,.T.);
#518=FACE_OUTER_BOUND('',#766,.T.);
#519=EDGE_LOOP('',(#1976,#1977,#1978,#1979));
#520=EDGE_LOOP('',(#1980,#1981,#1982,#1983));
#521=EDGE_LOOP('',(#1984,#1985,#1986,#1987));
#522=EDGE_LOOP('',(#1988,#1989,#1990,#1991));
#523=EDGE_LOOP('',(#1992,#1993,#1994,#1995));
#524=EDGE_LOOP('',(#1996,#1997,#1998,#1999));
#525=EDGE_LOOP('',(#2000,#2001,#2002,#2003));
#526=EDGE_LOOP('',(#2004,#2005,#2006,#2007));
#527=EDGE_LOOP('',(#2008,#2009,#2010,#2011));
#528=EDGE_LOOP('',(#2012,#2013,#2014,#2015));
#529=EDGE_LOOP('',(#2016,#2017,#2018,#2019));
#530=EDGE_LOOP('',(#2020,#2021,#2022,#2023));
#531=EDGE_LOOP('',(#2024,#2025,#2026,#2027));
#532=EDGE_LOOP('',(#2028,#2029,#2030,#2031));
#533=EDGE_LOOP('',(#2032,#2033,#2034,#2035));
#534=EDGE_LOOP('',(#2036,#2037,#2038,#2039));
#535=EDGE_LOOP('',(#2040,#2041,#2042,#2043));
#536=EDGE_LOOP('',(#2044,#2045,#2046,#2047));
#537=EDGE_LOOP('',(#2048,#2049,#2050,#2051));
#538=EDGE_LOOP('',(#2052));
#539=EDGE_LOOP('',(#2053));
#540=EDGE_LOOP('',(#2054));
#541=EDGE_LOOP('',(#2055));
#542=EDGE_LOOP('',(#2056));
#543=EDGE_LOOP('',(#2057));
#544=EDGE_LOOP('',(#2058,#2059,#2060,#2061));
#545=EDGE_LOOP('',(#2062));
#546=EDGE_LOOP('',(#2063));
#547=EDGE_LOOP('',(#2064));
#548=EDGE_LOOP('',(#2065));
#549=EDGE_LOOP('',(#2066));
#550=EDGE_LOOP('',(#2067));
#551=EDGE_LOOP('',(#2068,#2069,#2070,#2071));
#552=EDGE_LOOP('',(#2072,#2073,#2074,#2075));
#553=EDGE_LOOP('',(#2076,#2077,#2078,#2079));
#554=EDGE_LOOP('',(#2080,#2081,#2082,#2083));
#555=EDGE_LOOP('',(#2084,#2085,#2086,#2087));
#556=EDGE_LOOP('',(#2088,#2089,#2090,#2091));
#557=EDGE_LOOP('',(#2092,#2093,#2094,#2095,#2096));
#558=EDGE_LOOP('',(#2097,#2098,#2099,#2100,#2101));
#559=EDGE_LOOP('',(#2102,#2103,#2104,#2105));
#560=EDGE_LOOP('',(#2106,#2107,#2108,#2109));
#561=EDGE_LOOP('',(#2110,#2111,#2112,#2113));
#562=EDGE_LOOP('',(#2114,#2115,#2116,#2117));
#563=EDGE_LOOP('',(#2118,#2119,#2120,#2121));
#564=EDGE_LOOP('',(#2122,#2123,#2124,#2125));
#565=EDGE_LOOP('',(#2126,#2127,#2128,#2129));
#566=EDGE_LOOP('',(#2130,#2131));
#567=EDGE_LOOP('',(#2132,#2133));
#568=EDGE_LOOP('',(#2134,#2135,#2136,#2137));
#569=EDGE_LOOP('',(#2138,#2139,#2140,#2141));
#570=EDGE_LOOP('',(#2142));
#571=EDGE_LOOP('',(#2143));
#572=EDGE_LOOP('',(#2144));
#573=EDGE_LOOP('',(#2145));
#574=EDGE_LOOP('',(#2146));
#575=EDGE_LOOP('',(#2147));
#576=EDGE_LOOP('',(#2148));
#577=EDGE_LOOP('',(#2149));
#578=EDGE_LOOP('',(#2150));
#579=EDGE_LOOP('',(#2151));
#580=EDGE_LOOP('',(#2152));
#581=EDGE_LOOP('',(#2153));
#582=EDGE_LOOP('',(#2154));
#583=EDGE_LOOP('',(#2155));
#584=EDGE_LOOP('',(#2156));
#585=EDGE_LOOP('',(#2157));
#586=EDGE_LOOP('',(#2158,#2159,#2160,#2161));
#587=EDGE_LOOP('',(#2162,#2163,#2164,#2165));
#588=EDGE_LOOP('',(#2166,#2167,#2168,#2169));
#589=EDGE_LOOP('',(#2170,#2171,#2172));
#590=EDGE_LOOP('',(#2173,#2174,#2175,#2176));
#591=EDGE_LOOP('',(#2177,#2178,#2179,#2180));
#592=EDGE_LOOP('',(#2181,#2182,#2183,#2184));
#593=EDGE_LOOP('',(#2185,#2186,#2187,#2188));
#594=EDGE_LOOP('',(#2189,#2190,#2191,#2192));
#595=EDGE_LOOP('',(#2193,#2194,#2195,#2196));
#596=EDGE_LOOP('',(#2197,#2198,#2199,#2200));
#597=EDGE_LOOP('',(#2201,#2202,#2203,#2204));
#598=EDGE_LOOP('',(#2205,#2206,#2207,#2208));
#599=EDGE_LOOP('',(#2209,#2210,#2211,#2212));
#600=EDGE_LOOP('',(#2213,#2214,#2215,#2216));
#601=EDGE_LOOP('',(#2217,#2218,#2219,#2220));
#602=EDGE_LOOP('',(#2221,#2222,#2223,#2224,#2225,#2226,#2227,#2228));
#603=EDGE_LOOP('',(#2229,#2230,#2231,#2232));
#604=EDGE_LOOP('',(#2233,#2234,#2235,#2236));
#605=EDGE_LOOP('',(#2237,#2238,#2239,#2240,#2241,#2242,#2243,#2244));
#606=EDGE_LOOP('',(#2245));
#607=EDGE_LOOP('',(#2246));
#608=EDGE_LOOP('',(#2247));
#609=EDGE_LOOP('',(#2248,#2249,#2250,#2251));
#610=EDGE_LOOP('',(#2252,#2253,#2254,#2255));
#611=EDGE_LOOP('',(#2256,#2257,#2258,#2259));
#612=EDGE_LOOP('',(#2260,#2261,#2262,#2263));
#613=EDGE_LOOP('',(#2264));
#614=EDGE_LOOP('',(#2265,#2266,#2267,#2268));
#615=EDGE_LOOP('',(#2269));
#616=EDGE_LOOP('',(#2270,#2271,#2272,#2273));
#617=EDGE_LOOP('',(#2274));
#618=EDGE_LOOP('',(#2275,#2276,#2277,#2278));
#619=EDGE_LOOP('',(#2279));
#620=EDGE_LOOP('',(#2280,#2281,#2282,#2283));
#621=EDGE_LOOP('',(#2284,#2285,#2286,#2287,#2288,#2289));
#622=EDGE_LOOP('',(#2290,#2291,#2292,#2293,#2294,#2295));
#623=EDGE_LOOP('',(#2296,#2297,#2298,#2299,#2300,#2301));
#624=EDGE_LOOP('',(#2302,#2303,#2304,#2305,#2306,#2307));
#625=EDGE_LOOP('',(#2308,#2309,#2310,#2311,#2312,#2313));
#626=EDGE_LOOP('',(#2314,#2315,#2316,#2317,#2318,#2319));
#627=EDGE_LOOP('',(#2320,#2321,#2322,#2323,#2324,#2325));
#628=EDGE_LOOP('',(#2326));
#629=EDGE_LOOP('',(#2327,#2328,#2329,#2330,#2331,#2332));
#630=EDGE_LOOP('',(#2333));
#631=EDGE_LOOP('',(#2334,#2335,#2336));
#632=EDGE_LOOP('',(#2337,#2338,#2339));
#633=EDGE_LOOP('',(#2340,#2341,#2342));
#634=EDGE_LOOP('',(#2343,#2344,#2345));
#635=EDGE_LOOP('',(#2346,#2347,#2348));
#636=EDGE_LOOP('',(#2349,#2350,#2351));
#637=EDGE_LOOP('',(#2352,#2353,#2354));
#638=EDGE_LOOP('',(#2355,#2356,#2357));
#639=EDGE_LOOP('',(#2358,#2359,#2360));
#640=EDGE_LOOP('',(#2361,#2362,#2363));
#641=EDGE_LOOP('',(#2364,#2365,#2366));
#642=EDGE_LOOP('',(#2367,#2368,#2369));
#643=EDGE_LOOP('',(#2370,#2371,#2372,#2373));
#644=EDGE_LOOP('',(#2374,#2375,#2376,#2377,#2378,#2379));
#645=EDGE_LOOP('',(#2380,#2381,#2382,#2383,#2384,#2385));
#646=EDGE_LOOP('',(#2386,#2387,#2388,#2389,#2390,#2391));
#647=EDGE_LOOP('',(#2392,#2393,#2394,#2395,#2396,#2397));
#648=EDGE_LOOP('',(#2398,#2399,#2400,#2401,#2402,#2403));
#649=EDGE_LOOP('',(#2404,#2405,#2406,#2407,#2408,#2409));
#650=EDGE_LOOP('',(#2410,#2411,#2412,#2413,#2414,#2415));
#651=EDGE_LOOP('',(#2416));
#652=EDGE_LOOP('',(#2417,#2418,#2419,#2420,#2421,#2422));
#653=EDGE_LOOP('',(#2423));
#654=EDGE_LOOP('',(#2424,#2425,#2426));
#655=EDGE_LOOP('',(#2427,#2428,#2429));
#656=EDGE_LOOP('',(#2430,#2431,#2432));
#657=EDGE_LOOP('',(#2433,#2434,#2435));
#658=EDGE_LOOP('',(#2436,#2437,#2438));
#659=EDGE_LOOP('',(#2439,#2440,#2441));
#660=EDGE_LOOP('',(#2442,#2443,#2444));
#661=EDGE_LOOP('',(#2445,#2446,#2447));
#662=EDGE_LOOP('',(#2448,#2449,#2450));
#663=EDGE_LOOP('',(#2451,#2452,#2453));
#664=EDGE_LOOP('',(#2454,#2455,#2456));
#665=EDGE_LOOP('',(#2457,#2458,#2459));
#666=EDGE_LOOP('',(#2460,#2461,#2462,#2463));
#667=EDGE_LOOP('',(#2464,#2465,#2466,#2467));
#668=EDGE_LOOP('',(#2468,#2469,#2470,#2471));
#669=EDGE_LOOP('',(#2472,#2473,#2474,#2475));
#670=EDGE_LOOP('',(#2476,#2477,#2478,#2479));
#671=EDGE_LOOP('',(#2480,#2481,#2482,#2483));
#672=EDGE_LOOP('',(#2484,#2485,#2486,#2487));
#673=EDGE_LOOP('',(#2488,#2489,#2490,#2491));
#674=EDGE_LOOP('',(#2492,#2493,#2494,#2495));
#675=EDGE_LOOP('',(#2496,#2497,#2498,#2499));
#676=EDGE_LOOP('',(#2500,#2501,#2502,#2503));
#677=EDGE_LOOP('',(#2504,#2505,#2506,#2507));
#678=EDGE_LOOP('',(#2508,#2509,#2510,#2511));
#679=EDGE_LOOP('',(#2512));
#680=EDGE_LOOP('',(#2513));
#681=EDGE_LOOP('',(#2514,#2515,#2516,#2517));
#682=EDGE_LOOP('',(#2518));
#683=EDGE_LOOP('',(#2519));
#684=EDGE_LOOP('',(#2520,#2521,#2522,#2523));
#685=EDGE_LOOP('',(#2524));
#686=EDGE_LOOP('',(#2525));
#687=EDGE_LOOP('',(#2526,#2527,#2528,#2529));
#688=EDGE_LOOP('',(#2530));
#689=EDGE_LOOP('',(#2531));
#690=EDGE_LOOP('',(#2532,#2533,#2534,#2535));
#691=EDGE_LOOP('',(#2536));
#692=EDGE_LOOP('',(#2537));
#693=EDGE_LOOP('',(#2538,#2539,#2540,#2541));
#694=EDGE_LOOP('',(#2542));
#695=EDGE_LOOP('',(#2543));
#696=EDGE_LOOP('',(#2544,#2545,#2546,#2547));
#697=EDGE_LOOP('',(#2548));
#698=EDGE_LOOP('',(#2549));
#699=EDGE_LOOP('',(#2550,#2551,#2552,#2553));
#700=EDGE_LOOP('',(#2554));
#701=EDGE_LOOP('',(#2555));
#702=EDGE_LOOP('',(#2556,#2557,#2558,#2559,#2560));
#703=EDGE_LOOP('',(#2561,#2562,#2563,#2564,#2565));
#704=EDGE_LOOP('',(#2566,#2567,#2568,#2569));
#705=EDGE_LOOP('',(#2570,#2571,#2572,#2573));
#706=EDGE_LOOP('',(#2574,#2575,#2576,#2577,#2578));
#707=EDGE_LOOP('',(#2579,#2580,#2581,#2582));
#708=EDGE_LOOP('',(#2583,#2584,#2585,#2586,#2587));
#709=EDGE_LOOP('',(#2588));
#710=EDGE_LOOP('',(#2589));
#711=EDGE_LOOP('',(#2590));
#712=EDGE_LOOP('',(#2591));
#713=EDGE_LOOP('',(#2592));
#714=EDGE_LOOP('',(#2593));
#715=EDGE_LOOP('',(#2594,#2595,#2596,#2597,#2598,#2599,#2600,#2601));
#716=EDGE_LOOP('',(#2602,#2603,#2604,#2605,#2606));
#717=EDGE_LOOP('',(#2607,#2608,#2609,#2610,#2611));
#718=EDGE_LOOP('',(#2612,#2613,#2614,#2615,#2616));
#719=EDGE_LOOP('',(#2617,#2618,#2619,#2620,#2621));
#720=EDGE_LOOP('',(#2622,#2623,#2624,#2625));
#721=EDGE_LOOP('',(#2626));
#722=EDGE_LOOP('',(#2627,#2628,#2629,#2630,#2631,#2632));
#723=EDGE_LOOP('',(#2633));
#724=EDGE_LOOP('',(#2634));
#725=EDGE_LOOP('',(#2635));
#726=EDGE_LOOP('',(#2636,#2637,#2638,#2639,#2640));
#727=EDGE_LOOP('',(#2641,#2642,#2643,#2644,#2645));
#728=EDGE_LOOP('',(#2646,#2647,#2648,#2649,#2650));
#729=EDGE_LOOP('',(#2651,#2652,#2653,#2654,#2655));
#730=EDGE_LOOP('',(#2656,#2657,#2658,#2659,#2660));
#731=EDGE_LOOP('',(#2661,#2662,#2663,#2664,#2665));
#732=EDGE_LOOP('',(#2666,#2667,#2668));
#733=EDGE_LOOP('',(#2669,#2670,#2671));
#734=EDGE_LOOP('',(#2672,#2673,#2674));
#735=EDGE_LOOP('',(#2675,#2676,#2677));
#736=EDGE_LOOP('',(#2678,#2679,#2680));
#737=EDGE_LOOP('',(#2681,#2682,#2683));
#738=EDGE_LOOP('',(#2684,#2685,#2686,#2687));
#739=EDGE_LOOP('',(#2688,#2689,#2690,#2691));
#740=EDGE_LOOP('',(#2692));
#741=EDGE_LOOP('',(#2693));
#742=EDGE_LOOP('',(#2694));
#743=EDGE_LOOP('',(#2695));
#744=EDGE_LOOP('',(#2696,#2697,#2698,#2699,#2700,#2701,#2702,#2703));
#745=EDGE_LOOP('',(#2704,#2705,#2706,#2707,#2708));
#746=EDGE_LOOP('',(#2709,#2710,#2711,#2712));
#747=EDGE_LOOP('',(#2713,#2714,#2715,#2716,#2717));
#748=EDGE_LOOP('',(#2718,#2719,#2720,#2721,#2722));
#749=EDGE_LOOP('',(#2723,#2724,#2725,#2726,#2727));
#750=EDGE_LOOP('',(#2728));
#751=EDGE_LOOP('',(#2729,#2730,#2731,#2732,#2733,#2734));
#752=EDGE_LOOP('',(#2735));
#753=EDGE_LOOP('',(#2736));
#754=EDGE_LOOP('',(#2737));
#755=EDGE_LOOP('',(#2738,#2739,#2740,#2741,#2742));
#756=EDGE_LOOP('',(#2743,#2744,#2745,#2746,#2747));
#757=EDGE_LOOP('',(#2748,#2749,#2750,#2751,#2752));
#758=EDGE_LOOP('',(#2753,#2754,#2755,#2756,#2757));
#759=EDGE_LOOP('',(#2758,#2759,#2760,#2761,#2762));
#760=EDGE_LOOP('',(#2763,#2764,#2765,#2766,#2767));
#761=EDGE_LOOP('',(#2768,#2769,#2770));
#762=EDGE_LOOP('',(#2771,#2772,#2773));
#763=EDGE_LOOP('',(#2774,#2775,#2776));
#764=EDGE_LOOP('',(#2777,#2778,#2779));
#765=EDGE_LOOP('',(#2780,#2781,#2782));
#766=EDGE_LOOP('',(#2783,#2784,#2785));
#767=LINE('',#4494,#963);
#768=LINE('',#4497,#964);
#769=LINE('',#4500,#965);
#770=LINE('',#4504,#966);
#771=LINE('',#4511,#967);
#772=LINE('',#4514,#968);
#773=LINE('',#4519,#969);
#774=LINE('',#4522,#970);
#775=LINE('',#4524,#971);
#776=LINE('',#4525,#972);
#777=LINE('',#4527,#973);
#778=LINE('',#4529,#974);
#779=LINE('',#4532,#975);
#780=LINE('',#4533,#976);
#781=LINE('',#4535,#977);
#782=LINE('',#4537,#978);
#783=LINE('',#4544,#979);
#784=LINE('',#4550,#980);
#785=LINE('',#4556,#981);
#786=LINE('',#4562,#982);
#787=LINE('',#4568,#983);
#788=LINE('',#4574,#984);
#789=LINE('',#4579,#985);
#790=LINE('',#4581,#986);
#791=LINE('',#4584,#987);
#792=LINE('',#4588,#988);
#793=LINE('',#4590,#989);
#794=LINE('',#4593,#990);
#795=LINE('',#4595,#991);
#796=LINE('',#4596,#992);
#797=LINE('',#4598,#993);
#798=LINE('',#4600,#994);
#799=LINE('',#4652,#995);
#800=LINE('',#4724,#996);
#801=LINE('',#4785,#997);
#802=LINE('',#4791,#998);
#803=LINE('',#4797,#999);
#804=LINE('',#4803,#1000);
#805=LINE('',#4809,#1001);
#806=LINE('',#4813,#1002);
#807=LINE('',#4818,#1003);
#808=LINE('',#4822,#1004);
#809=LINE('',#4825,#1005);
#810=LINE('',#4836,#1006);
#811=LINE('',#4842,#1007);
#812=LINE('',#4848,#1008);
#813=LINE('',#4884,#1009);
#814=LINE('',#4890,#1010);
#815=LINE('',#4893,#1011);
#816=LINE('',#4896,#1012);
#817=LINE('',#4898,#1013);
#818=LINE('',#4899,#1014);
#819=LINE('',#4902,#1015);
#820=LINE('',#4904,#1016);
#821=LINE('',#4905,#1017);
#822=LINE('',#4911,#1018);
#823=LINE('',#4914,#1019);
#824=LINE('',#4917,#1020);
#825=LINE('',#4919,#1021);
#826=LINE('',#4920,#1022);
#827=LINE('',#4925,#1023);
#828=LINE('',#4929,#1024);
#829=LINE('',#4931,#1025);
#830=LINE('',#4932,#1026);
#831=LINE('',#4937,#1027);
#832=LINE('',#4941,#1028);
#833=LINE('',#4943,#1029);
#834=LINE('',#4944,#1030);
#835=LINE('',#4949,#1031);
#836=LINE('',#4952,#1032);
#837=LINE('',#4953,#1033);
#838=LINE('',#4957,#1034);
#839=LINE('',#4959,#1035);
#840=LINE('',#4961,#1036);
#841=LINE('',#4962,#1037);
#842=LINE('',#4963,#1038);
#843=LINE('',#4964,#1039);
#844=LINE('',#4970,#1040);
#845=LINE('',#4974,#1041);
#846=LINE('',#4977,#1042);
#847=LINE('',#4978,#1043);
#848=LINE('',#4980,#1044);
#849=LINE('',#4981,#1045);
#850=LINE('',#4991,#1046);
#851=LINE('',#4996,#1047);
#852=LINE('',#5006,#1048);
#853=LINE('',#5024,#1049);
#854=LINE('',#5039,#1050);
#855=LINE('',#5060,#1051);
#856=LINE('',#5078,#1052);
#857=LINE('',#5132,#1053);
#858=LINE('',#5137,#1054);
#859=LINE('',#5147,#1055);
#860=LINE('',#5165,#1056);
#861=LINE('',#5180,#1057);
#862=LINE('',#5201,#1058);
#863=LINE('',#5219,#1059);
#864=LINE('',#5273,#1060);
#865=LINE('',#5279,#1061);
#866=LINE('',#5285,#1062);
#867=LINE('',#5291,#1063);
#868=LINE('',#5297,#1064);
#869=LINE('',#5303,#1065);
#870=LINE('',#5309,#1066);
#871=LINE('',#5315,#1067);
#872=LINE('',#5320,#1068);
#873=LINE('',#5322,#1069);
#874=LINE('',#5324,#1070);
#875=LINE('',#5325,#1071);
#876=LINE('',#5328,#1072);
#877=LINE('',#5330,#1073);
#878=LINE('',#5332,#1074);
#879=LINE('',#5333,#1075);
#880=LINE('',#5337,#1076);
#881=LINE('',#5339,#1077);
#882=LINE('',#5341,#1078);
#883=LINE('',#5342,#1079);
#884=LINE('',#5345,#1080);
#885=LINE('',#5347,#1081);
#886=LINE('',#5349,#1082);
#887=LINE('',#5350,#1083);
#888=LINE('',#5352,#1084);
#889=LINE('',#5353,#1085);
#890=LINE('',#5355,#1086);
#891=LINE('',#5357,#1087);
#892=LINE('',#5360,#1088);
#893=LINE('',#5361,#1089);
#894=LINE('',#5363,#1090);
#895=LINE('',#5365,#1091);
#896=LINE('',#5374,#1092);
#897=LINE('',#5382,#1093);
#898=LINE('',#5388,#1094);
#899=LINE('',#5394,#1095);
#900=LINE('',#5397,#1096);
#901=LINE('',#5401,#1097);
#902=LINE('',#5404,#1098);
#903=LINE('',#5414,#1099);
#904=LINE('',#5439,#1100);
#905=LINE('',#5444,#1101);
#906=LINE('',#5448,#1102);
#907=LINE('',#5452,#1103);
#908=LINE('',#5457,#1104);
#909=LINE('',#5459,#1105);
#910=LINE('',#5461,#1106);
#911=LINE('',#5463,#1107);
#912=LINE('',#5465,#1108);
#913=LINE('',#5466,#1109);
#914=LINE('',#5471,#1110);
#915=LINE('',#5472,#1111);
#916=LINE('',#5474,#1112);
#917=LINE('',#5475,#1113);
#918=LINE('',#5477,#1114);
#919=LINE('',#5479,#1115);
#920=LINE('',#5480,#1116);
#921=LINE('',#5482,#1117);
#922=LINE('',#5484,#1118);
#923=LINE('',#5485,#1119);
#924=LINE('',#5487,#1120);
#925=LINE('',#5489,#1121);
#926=LINE('',#5490,#1122);
#927=LINE('',#5492,#1123);
#928=LINE('',#5494,#1124);
#929=LINE('',#5495,#1125);
#930=LINE('',#5497,#1126);
#931=LINE('',#5498,#1127);
#932=LINE('',#5510,#1128);
#933=LINE('',#5516,#1129);
#934=LINE('',#5524,#1130);
#935=LINE('',#5548,#1131);
#936=LINE('',#5551,#1132);
#937=LINE('',#5558,#1133);
#938=LINE('',#5562,#1134);
#939=LINE('',#5567,#1135);
#940=LINE('',#5569,#1136);
#941=LINE('',#5571,#1137);
#942=LINE('',#5573,#1138);
#943=LINE('',#5575,#1139);
#944=LINE('',#5576,#1140);
#945=LINE('',#5581,#1141);
#946=LINE('',#5582,#1142);
#947=LINE('',#5584,#1143);
#948=LINE('',#5585,#1144);
#949=LINE('',#5587,#1145);
#950=LINE('',#5589,#1146);
#951=LINE('',#5590,#1147);
#952=LINE('',#5592,#1148);
#953=LINE('',#5594,#1149);
#954=LINE('',#5595,#1150);
#955=LINE('',#5597,#1151);
#956=LINE('',#5599,#1152);
#957=LINE('',#5600,#1153);
#958=LINE('',#5602,#1154);
#959=LINE('',#5604,#1155);
#960=LINE('',#5605,#1156);
#961=LINE('',#5607,#1157);
#962=LINE('',#5608,#1158);
#963=VECTOR('',#3567,1000.);
#964=VECTOR('',#3570,1000.);
#965=VECTOR('',#3571,1000.);
#966=VECTOR('',#3574,1000.);
#967=VECTOR('',#3581,1000.);
#968=VECTOR('',#3584,1000.);
#969=VECTOR('',#3587,1000.);
#970=VECTOR('',#3590,1000.);
#971=VECTOR('',#3593,1000.);
#972=VECTOR('',#3594,1000.);
#973=VECTOR('',#3597,1000.);
#974=VECTOR('',#3600,1000.);
#975=VECTOR('',#3605,1000.);
#976=VECTOR('',#3606,1000.);
#977=VECTOR('',#3609,1000.);
#978=VECTOR('',#3612,1000.);
#979=VECTOR('',#3621,4.);
#980=VECTOR('',#3628,4.);
#981=VECTOR('',#3635,4.);
#982=VECTOR('',#3642,3.99999999999999);
#983=VECTOR('',#3649,5.75);
#984=VECTOR('',#3656,5.75000000000001);
#985=VECTOR('',#3661,1000.);
#986=VECTOR('',#3662,1000.);
#987=VECTOR('',#3665,1000.);
#988=VECTOR('',#3668,1000.);
#989=VECTOR('',#3669,1000.);
#990=VECTOR('',#3672,1000.);
#991=VECTOR('',#3675,1000.);
#992=VECTOR('',#3676,1000.);
#993=VECTOR('',#3679,1000.);
#994=VECTOR('',#3682,1000.);
#995=VECTOR('',#3705,5.50000000000001);
#996=VECTOR('',#3708,5.50000000000001);
#997=VECTOR('',#3713,4.);
#998=VECTOR('',#3720,4.);
#999=VECTOR('',#3727,4.);
#1000=VECTOR('',#3734,4.00000000000001);
#1001=VECTOR('',#3741,50.);
#1002=VECTOR('',#3746,7.);
#1003=VECTOR('',#3753,7.00000000000001);
#1004=VECTOR('',#3758,10.);
#1005=VECTOR('',#3761,10.);
#1006=VECTOR('',#3778,5.5);
#1007=VECTOR('',#3785,5.5);
#1008=VECTOR('',#3792,35.);
#1009=VECTOR('',#3803,32.5);
#1010=VECTOR('',#3808,1000.);
#1011=VECTOR('',#3811,1000.);
#1012=VECTOR('',#3814,1000.);
#1013=VECTOR('',#3815,1000.);
#1014=VECTOR('',#3816,1000.);
#1015=VECTOR('',#3819,1000.);
#1016=VECTOR('',#3820,1000.);
#1017=VECTOR('',#3821,1000.);
#1018=VECTOR('',#3826,1000.);
#1019=VECTOR('',#3829,1000.);
#1020=VECTOR('',#3832,1000.);
#1021=VECTOR('',#3833,1000.);
#1022=VECTOR('',#3834,1000.);
#1023=VECTOR('',#3839,1000.);
#1024=VECTOR('',#3844,1000.);
#1025=VECTOR('',#3845,1000.);
#1026=VECTOR('',#3846,1000.);
#1027=VECTOR('',#3851,1000.);
#1028=VECTOR('',#3856,1000.);
#1029=VECTOR('',#3857,1000.);
#1030=VECTOR('',#3858,1000.);
#1031=VECTOR('',#3863,1000.);
#1032=VECTOR('',#3868,1000.);
#1033=VECTOR('',#3869,1000.);
#1034=VECTOR('',#3872,1000.);
#1035=VECTOR('',#3873,1000.);
#1036=VECTOR('',#3874,1000.);
#1037=VECTOR('',#3875,1000.);
#1038=VECTOR('',#3876,1000.);
#1039=VECTOR('',#3877,1000.);
#1040=VECTOR('',#3884,1000.);
#1041=VECTOR('',#3887,1000.);
#1042=VECTOR('',#3892,1000.);
#1043=VECTOR('',#3893,1000.);
#1044=VECTOR('',#3896,1000.);
#1045=VECTOR('',#3897,1000.);
#1046=VECTOR('',#3912,5.);
#1047=VECTOR('',#3917,1000.);
#1048=VECTOR('',#3918,1000.);
#1049=VECTOR('',#3921,1000.);
#1050=VECTOR('',#3924,1000.);
#1051=VECTOR('',#3927,1000.);
#1052=VECTOR('',#3930,1000.);
#1053=VECTOR('',#3991,5.);
#1054=VECTOR('',#3996,1000.);
#1055=VECTOR('',#3997,1000.);
#1056=VECTOR('',#4000,1000.);
#1057=VECTOR('',#4003,1000.);
#1058=VECTOR('',#4006,1000.);
#1059=VECTOR('',#4009,1000.);
#1060=VECTOR('',#4070,5.);
#1061=VECTOR('',#4077,5.);
#1062=VECTOR('',#4084,5.);
#1063=VECTOR('',#4091,5.);
#1064=VECTOR('',#4098,25.);
#1065=VECTOR('',#4105,25.);
#1066=VECTOR('',#4112,25.);
#1067=VECTOR('',#4119,25.);
#1068=VECTOR('',#4124,1000.);
#1069=VECTOR('',#4125,1000.);
#1070=VECTOR('',#4126,1000.);
#1071=VECTOR('',#4127,1000.);
#1072=VECTOR('',#4128,1000.);
#1073=VECTOR('',#4129,1000.);
#1074=VECTOR('',#4130,1000.);
#1075=VECTOR('',#4131,1000.);
#1076=VECTOR('',#4134,1000.);
#1077=VECTOR('',#4135,1000.);
#1078=VECTOR('',#4136,1000.);
#1079=VECTOR('',#4137,1000.);
#1080=VECTOR('',#4138,1000.);
#1081=VECTOR('',#4139,1000.);
#1082=VECTOR('',#4140,1000.);
#1083=VECTOR('',#4141,1000.);
#1084=VECTOR('',#4144,1000.);
#1085=VECTOR('',#4145,1000.);
#1086=VECTOR('',#4148,1000.);
#1087=VECTOR('',#4151,1000.);
#1088=VECTOR('',#4156,1000.);
#1089=VECTOR('',#4157,1000.);
#1090=VECTOR('',#4160,1000.);
#1091=VECTOR('',#4163,1000.);
#1092=VECTOR('',#4174,70.0000000000001);
#1093=VECTOR('',#4183,19.5);
#1094=VECTOR('',#4190,24.5);
#1095=VECTOR('',#4197,75.);
#1096=VECTOR('',#4202,75.);
#1097=VECTOR('',#4207,24.5);
#1098=VECTOR('',#4210,24.5);
#1099=VECTOR('',#4225,4.0575);
#1100=VECTOR('',#4252,7.);
#1101=VECTOR('',#4259,8.);
#1102=VECTOR('',#4264,5.00000000000003);
#1103=VECTOR('',#4269,4.172);
#1104=VECTOR('',#4274,1000.);
#1105=VECTOR('',#4275,1000.);
#1106=VECTOR('',#4276,1000.);
#1107=VECTOR('',#4277,1000.);
#1108=VECTOR('',#4278,1000.);
#1109=VECTOR('',#4279,1000.);
#1110=VECTOR('',#4286,1000.);
#1111=VECTOR('',#4287,1000.);
#1112=VECTOR('',#4288,1000.);
#1113=VECTOR('',#4289,1000.);
#1114=VECTOR('',#4292,1000.);
#1115=VECTOR('',#4293,1000.);
#1116=VECTOR('',#4294,1000.);
#1117=VECTOR('',#4297,1000.);
#1118=VECTOR('',#4298,1000.);
#1119=VECTOR('',#4299,1000.);
#1120=VECTOR('',#4302,1000.);
#1121=VECTOR('',#4303,1000.);
#1122=VECTOR('',#4304,1000.);
#1123=VECTOR('',#4307,1000.);
#1124=VECTOR('',#4308,1000.);
#1125=VECTOR('',#4309,1000.);
#1126=VECTOR('',#4312,1000.);
#1127=VECTOR('',#4313,1000.);
#1128=VECTOR('',#4332,10.);
#1129=VECTOR('',#4339,5.56);
#1130=VECTOR('',#4350,3.0475);
#1131=VECTOR('',#4377,3.3095);
#1132=VECTOR('',#4382,4.00000000000003);
#1133=VECTOR('',#4389,6.5);
#1134=VECTOR('',#4394,5.7);
#1135=VECTOR('',#4399,1000.);
#1136=VECTOR('',#4400,1000.);
#1137=VECTOR('',#4401,1000.);
#1138=VECTOR('',#4402,1000.);
#1139=VECTOR('',#4403,1000.);
#1140=VECTOR('',#4404,1000.);
#1141=VECTOR('',#4411,1000.);
#1142=VECTOR('',#4412,1000.);
#1143=VECTOR('',#4413,1000.);
#1144=VECTOR('',#4414,1000.);
#1145=VECTOR('',#4417,1000.);
#1146=VECTOR('',#4418,1000.);
#1147=VECTOR('',#4419,1000.);
#1148=VECTOR('',#4422,1000.);
#1149=VECTOR('',#4423,1000.);
#1150=VECTOR('',#4424,1000.);
#1151=VECTOR('',#4427,1000.);
#1152=VECTOR('',#4428,1000.);
#1153=VECTOR('',#4429,1000.);
#1154=VECTOR('',#4432,1000.);
#1155=VECTOR('',#4433,1000.);
#1156=VECTOR('',#4434,1000.);
#1157=VECTOR('',#4437,1000.);
#1158=VECTOR('',#4438,1000.);
#1159=CIRCLE('',#3196,80.);
#1160=CIRCLE('',#3197,80.);
#1161=CIRCLE('',#3198,75.);
#1162=CIRCLE('',#3199,75.);
#1163=CIRCLE('',#3201,80.);
#1164=CIRCLE('',#3202,80.);
#1165=CIRCLE('',#3203,75.);
#1166=CIRCLE('',#3204,75.);
#1167=CIRCLE('',#3215,4.);
#1168=CIRCLE('',#3216,4.);
#1169=CIRCLE('',#3218,4.);
#1170=CIRCLE('',#3219,4.);
#1171=CIRCLE('',#3221,4.00000000000001);
#1172=CIRCLE('',#3222,4.00000000000001);
#1173=CIRCLE('',#3224,3.99999999999999);
#1174=CIRCLE('',#3225,3.99999999999999);
#1175=CIRCLE('',#3227,5.75);
#1176=CIRCLE('',#3228,5.75);
#1177=CIRCLE('',#3230,5.75000000000001);
#1178=CIRCLE('',#3231,5.75000000000001);
#1179=CIRCLE('',#3233,50.0000000000001);
#1180=CIRCLE('',#3235,50.0000000000001);
#1181=CIRCLE('',#3242,7.00000000000001);
#1182=CIRCLE('',#3243,23.);
#1183=CIRCLE('',#3244,7.);
#1184=CIRCLE('',#3246,10.);
#1185=CIRCLE('',#3247,20.);
#1186=CIRCLE('',#3248,10.);
#1187=CIRCLE('',#3252,4.);
#1188=CIRCLE('',#3253,4.);
#1189=CIRCLE('',#3255,4.);
#1190=CIRCLE('',#3256,4.);
#1191=CIRCLE('',#3258,4.);
#1192=CIRCLE('',#3259,4.);
#1193=CIRCLE('',#3261,4.00000000000001);
#1194=CIRCLE('',#3262,4.00000000000001);
#1195=CIRCLE('',#3264,50.);
#1196=CIRCLE('',#3265,50.);
#1197=CIRCLE('',#3267,7.);
#1198=CIRCLE('',#3269,7.00000000000001);
#1199=CIRCLE('',#3271,10.);
#1200=CIRCLE('',#3273,10.);
#1201=CIRCLE('',#3280,5.5);
#1202=CIRCLE('',#3281,5.5);
#1203=CIRCLE('',#3283,5.5);
#1204=CIRCLE('',#3284,5.5);
#1205=CIRCLE('',#3286,35.);
#1206=CIRCLE('',#3287,35.);
#1207=CIRCLE('',#3288,32.5);
#1208=CIRCLE('',#3289,70.);
#1209=CIRCLE('',#3291,32.5);
#1210=CIRCLE('',#3293,15.);
#1211=CIRCLE('',#3294,15.);
#1212=CIRCLE('',#3298,20.);
#1213=CIRCLE('',#3299,20.);
#1214=CIRCLE('',#3302,20.);
#1215=CIRCLE('',#3303,20.);
#1216=CIRCLE('',#3306,20.);
#1217=CIRCLE('',#3307,20.);
#1218=CIRCLE('',#3310,20.);
#1219=CIRCLE('',#3311,20.);
#1220=CIRCLE('',#3317,15.);
#1221=CIRCLE('',#3318,15.);
#1222=CIRCLE('',#3327,5.);
#1223=CIRCLE('',#3328,4.99999999999999);
#1224=CIRCLE('',#3336,8.);
#1225=CIRCLE('',#3337,8.);
#1226=CIRCLE('',#3338,8.);
#1227=CIRCLE('',#3339,8.);
#1228=CIRCLE('',#3340,8.);
#1229=CIRCLE('',#3341,8.);
#1230=CIRCLE('',#3343,8.);
#1231=CIRCLE('',#3344,8.);
#1232=CIRCLE('',#3345,8.);
#1233=CIRCLE('',#3346,8.);
#1234=CIRCLE('',#3347,8.);
#1235=CIRCLE('',#3348,8.);
#1236=CIRCLE('',#3363,5.);
#1237=CIRCLE('',#3364,4.99999999999999);
#1238=CIRCLE('',#3372,8.);
#1239=CIRCLE('',#3373,8.);
#1240=CIRCLE('',#3374,8.);
#1241=CIRCLE('',#3375,8.);
#1242=CIRCLE('',#3376,8.);
#1243=CIRCLE('',#3377,8.);
#1244=CIRCLE('',#3379,8.);
#1245=CIRCLE('',#3380,8.);
#1246=CIRCLE('',#3381,8.);
#1247=CIRCLE('',#3382,8.);
#1248=CIRCLE('',#3383,8.);
#1249=CIRCLE('',#3384,8.);
#1250=CIRCLE('',#3399,5.);
#1251=CIRCLE('',#3400,5.);
#1252=CIRCLE('',#3402,5.);
#1253=CIRCLE('',#3403,5.);
#1254=CIRCLE('',#3405,5.);
#1255=CIRCLE('',#3406,5.);
#1256=CIRCLE('',#3408,5.);
#1257=CIRCLE('',#3409,5.);
#1258=CIRCLE('',#3411,25.);
#1259=CIRCLE('',#3412,25.);
#1260=CIRCLE('',#3414,25.);
#1261=CIRCLE('',#3415,25.);
#1262=CIRCLE('',#3417,25.);
#1263=CIRCLE('',#3418,25.);
#1264=CIRCLE('',#3420,25.);
#1265=CIRCLE('',#3421,25.);
#1266=CIRCLE('',#3434,75.);
#1267=CIRCLE('',#3435,75.);
#1268=CIRCLE('',#3436,70.0000000000001);
#1269=CIRCLE('',#3438,24.5);
#1270=CIRCLE('',#3439,24.5);
#1271=CIRCLE('',#3440,19.5);
#1272=CIRCLE('',#3442,24.5);
#1273=CIRCLE('',#3443,19.5);
#1274=CIRCLE('',#3445,75.);
#1275=CIRCLE('',#3446,70.);
#1276=CIRCLE('',#3449,24.5);
#1277=CIRCLE('',#3451,24.5);
#1278=CIRCLE('',#3458,4.0575);
#1279=CIRCLE('',#3459,4.0575);
#1280=CIRCLE('',#3460,4.0575);
#1281=CIRCLE('',#3461,4.0575);
#1282=CIRCLE('',#3462,4.0575);
#1283=CIRCLE('',#3463,4.0575);
#1284=CIRCLE('',#3465,5.00000000000003);
#1285=CIRCLE('',#3466,5.00000000000003);
#1286=CIRCLE('',#3467,0.4);
#1287=CIRCLE('',#3468,5.40000000000003);
#1288=CIRCLE('',#3470,8.);
#1289=CIRCLE('',#3471,7.);
#1290=CIRCLE('',#3472,8.);
#1291=CIRCLE('',#3474,8.);
#1292=CIRCLE('',#3476,5.00000000000007);
#1293=CIRCLE('',#3478,4.172);
#1294=CIRCLE('',#3496,10.);
#1295=CIRCLE('',#3497,10.);
#1296=CIRCLE('',#3499,5.56);
#1297=CIRCLE('',#3500,5.56);
#1298=CIRCLE('',#3505,3.0475);
#1299=CIRCLE('',#3506,3.0475);
#1300=CIRCLE('',#3507,3.0475);
#1301=CIRCLE('',#3508,3.0475);
#1302=CIRCLE('',#3509,3.0475);
#1303=CIRCLE('',#3510,3.0475);
#1304=CIRCLE('',#3512,4.00000000000003);
#1305=CIRCLE('',#3513,4.00000000000003);
#1306=CIRCLE('',#3514,0.4);
#1307=CIRCLE('',#3515,4.40000000000003);
#1308=CIRCLE('',#3517,4.00000000000006);
#1309=CIRCLE('',#3518,3.3095);
#1310=CIRCLE('',#3521,6.5);
#1311=CIRCLE('',#3522,6.5);
#1312=CIRCLE('',#3523,6.5);
#1313=CIRCLE('',#3525,5.7);
#1314=VERTEX_POINT('',#4490);
#1315=VERTEX_POINT('',#4491);
#1316=VERTEX_POINT('',#4493);
#1317=VERTEX_POINT('',#4495);
#1318=VERTEX_POINT('',#4498);
#1319=VERTEX_POINT('',#4499);
#1320=VERTEX_POINT('',#4501);
#1321=VERTEX_POINT('',#4503);
#1322=VERTEX_POINT('',#4507);
#1323=VERTEX_POINT('',#4508);
#1324=VERTEX_POINT('',#4510);
#1325=VERTEX_POINT('',#4512);
#1326=VERTEX_POINT('',#4515);
#1327=VERTEX_POINT('',#4516);
#1328=VERTEX_POINT('',#4518);
#1329=VERTEX_POINT('',#4520);
#1330=VERTEX_POINT('',#4541);
#1331=VERTEX_POINT('',#4543);
#1332=VERTEX_POINT('',#4547);
#1333=VERTEX_POINT('',#4549);
#1334=VERTEX_POINT('',#4553);
#1335=VERTEX_POINT('',#4555);
#1336=VERTEX_POINT('',#4559);
#1337=VERTEX_POINT('',#4561);
#1338=VERTEX_POINT('',#4565);
#1339=VERTEX_POINT('',#4567);
#1340=VERTEX_POINT('',#4571);
#1341=VERTEX_POINT('',#4573);
#1342=VERTEX_POINT('',#4577);
#1343=VERTEX_POINT('',#4578);
#1344=VERTEX_POINT('',#4580);
#1345=VERTEX_POINT('',#4582);
#1346=VERTEX_POINT('',#4586);
#1347=VERTEX_POINT('',#4587);
#1348=VERTEX_POINT('',#4589);
#1349=VERTEX_POINT('',#4591);
#1350=VERTEX_POINT('',#4604);
#1351=VERTEX_POINT('',#4606);
#1352=VERTEX_POINT('',#4610);
#1353=VERTEX_POINT('',#4612);
#1354=VERTEX_POINT('',#4616);
#1355=VERTEX_POINT('',#4651);
#1356=VERTEX_POINT('',#4653);
#1357=VERTEX_POINT('',#4699);
#1358=VERTEX_POINT('',#4700);
#1359=VERTEX_POINT('',#4723);
#1360=VERTEX_POINT('',#4782);
#1361=VERTEX_POINT('',#4784);
#1362=VERTEX_POINT('',#4788);
#1363=VERTEX_POINT('',#4790);
#1364=VERTEX_POINT('',#4794);
#1365=VERTEX_POINT('',#4796);
#1366=VERTEX_POINT('',#4800);
#1367=VERTEX_POINT('',#4802);
#1368=VERTEX_POINT('',#4806);
#1369=VERTEX_POINT('',#4808);
#1370=VERTEX_POINT('',#4812);
#1371=VERTEX_POINT('',#4816);
#1372=VERTEX_POINT('',#4820);
#1373=VERTEX_POINT('',#4824);
#1374=VERTEX_POINT('',#4833);
#1375=VERTEX_POINT('',#4835);
#1376=VERTEX_POINT('',#4839);
#1377=VERTEX_POINT('',#4841);
#1378=VERTEX_POINT('',#4845);
#1379=VERTEX_POINT('',#4847);
#1380=VERTEX_POINT('',#4877);
#1381=VERTEX_POINT('',#4879);
#1382=VERTEX_POINT('',#4882);
#1383=VERTEX_POINT('',#4886);
#1384=VERTEX_POINT('',#4887);
#1385=VERTEX_POINT('',#4889);
#1386=VERTEX_POINT('',#4891);
#1387=VERTEX_POINT('',#4895);
#1388=VERTEX_POINT('',#4897);
#1389=VERTEX_POINT('',#4901);
#1390=VERTEX_POINT('',#4903);
#1391=VERTEX_POINT('',#4907);
#1392=VERTEX_POINT('',#4908);
#1393=VERTEX_POINT('',#4910);
#1394=VERTEX_POINT('',#4912);
#1395=VERTEX_POINT('',#4916);
#1396=VERTEX_POINT('',#4918);
#1397=VERTEX_POINT('',#4922);
#1398=VERTEX_POINT('',#4924);
#1399=VERTEX_POINT('',#4928);
#1400=VERTEX_POINT('',#4930);
#1401=VERTEX_POINT('',#4934);
#1402=VERTEX_POINT('',#4936);
#1403=VERTEX_POINT('',#4940);
#1404=VERTEX_POINT('',#4942);
#1405=VERTEX_POINT('',#4946);
#1406=VERTEX_POINT('',#4948);
#1407=VERTEX_POINT('',#4955);
#1408=VERTEX_POINT('',#4956);
#1409=VERTEX_POINT('',#4958);
#1410=VERTEX_POINT('',#4960);
#1411=VERTEX_POINT('',#4968);
#1412=VERTEX_POINT('',#4969);
#1413=VERTEX_POINT('',#4971);
#1414=VERTEX_POINT('',#4973);
#1415=VERTEX_POINT('',#4988);
#1416=VERTEX_POINT('',#4990);
#1417=VERTEX_POINT('',#4994);
#1418=VERTEX_POINT('',#4995);
#1419=VERTEX_POINT('',#4997);
#1420=VERTEX_POINT('',#5001);
#1421=VERTEX_POINT('',#5005);
#1422=VERTEX_POINT('',#5007);
#1423=VERTEX_POINT('',#5015);
#1424=VERTEX_POINT('',#5019);
#1425=VERTEX_POINT('',#5023);
#1426=VERTEX_POINT('',#5025);
#1427=VERTEX_POINT('',#5033);
#1428=VERTEX_POINT('',#5034);
#1429=VERTEX_POINT('',#5038);
#1430=VERTEX_POINT('',#5040);
#1431=VERTEX_POINT('',#5051);
#1432=VERTEX_POINT('',#5055);
#1433=VERTEX_POINT('',#5059);
#1434=VERTEX_POINT('',#5061);
#1435=VERTEX_POINT('',#5069);
#1436=VERTEX_POINT('',#5073);
#1437=VERTEX_POINT('',#5077);
#1438=VERTEX_POINT('',#5079);
#1439=VERTEX_POINT('',#5087);
#1440=VERTEX_POINT('',#5094);
#1441=VERTEX_POINT('',#5129);
#1442=VERTEX_POINT('',#5131);
#1443=VERTEX_POINT('',#5135);
#1444=VERTEX_POINT('',#5136);
#1445=VERTEX_POINT('',#5138);
#1446=VERTEX_POINT('',#5142);
#1447=VERTEX_POINT('',#5146);
#1448=VERTEX_POINT('',#5148);
#1449=VERTEX_POINT('',#5156);
#1450=VERTEX_POINT('',#5160);
#1451=VERTEX_POINT('',#5164);
#1452=VERTEX_POINT('',#5166);
#1453=VERTEX_POINT('',#5174);
#1454=VERTEX_POINT('',#5175);
#1455=VERTEX_POINT('',#5179);
#1456=VERTEX_POINT('',#5181);
#1457=VERTEX_POINT('',#5192);
#1458=VERTEX_POINT('',#5196);
#1459=VERTEX_POINT('',#5200);
#1460=VERTEX_POINT('',#5202);
#1461=VERTEX_POINT('',#5210);
#1462=VERTEX_POINT('',#5214);
#1463=VERTEX_POINT('',#5218);
#1464=VERTEX_POINT('',#5220);
#1465=VERTEX_POINT('',#5228);
#1466=VERTEX_POINT('',#5235);
#1467=VERTEX_POINT('',#5270);
#1468=VERTEX_POINT('',#5272);
#1469=VERTEX_POINT('',#5276);
#1470=VERTEX_POINT('',#5278);
#1471=VERTEX_POINT('',#5282);
#1472=VERTEX_POINT('',#5284);
#1473=VERTEX_POINT('',#5288);
#1474=VERTEX_POINT('',#5290);
#1475=VERTEX_POINT('',#5294);
#1476=VERTEX_POINT('',#5296);
#1477=VERTEX_POINT('',#5300);
#1478=VERTEX_POINT('',#5302);
#1479=VERTEX_POINT('',#5306);
#1480=VERTEX_POINT('',#5308);
#1481=VERTEX_POINT('',#5312);
#1482=VERTEX_POINT('',#5314);
#1483=VERTEX_POINT('',#5318);
#1484=VERTEX_POINT('',#5319);
#1485=VERTEX_POINT('',#5321);
#1486=VERTEX_POINT('',#5323);
#1487=VERTEX_POINT('',#5326);
#1488=VERTEX_POINT('',#5327);
#1489=VERTEX_POINT('',#5329);
#1490=VERTEX_POINT('',#5331);
#1491=VERTEX_POINT('',#5335);
#1492=VERTEX_POINT('',#5336);
#1493=VERTEX_POINT('',#5338);
#1494=VERTEX_POINT('',#5340);
#1495=VERTEX_POINT('',#5343);
#1496=VERTEX_POINT('',#5344);
#1497=VERTEX_POINT('',#5346);
#1498=VERTEX_POINT('',#5348);
#1499=VERTEX_POINT('',#5369);
#1500=VERTEX_POINT('',#5370);
#1501=VERTEX_POINT('',#5373);
#1502=VERTEX_POINT('',#5377);
#1503=VERTEX_POINT('',#5378);
#1504=VERTEX_POINT('',#5381);
#1505=VERTEX_POINT('',#5385);
#1506=VERTEX_POINT('',#5387);
#1507=VERTEX_POINT('',#5391);
#1508=VERTEX_POINT('',#5393);
#1509=VERTEX_POINT('',#5399);
#1510=VERTEX_POINT('',#5403);
#1511=VERTEX_POINT('',#5412);
#1512=VERTEX_POINT('',#5413);
#1513=VERTEX_POINT('',#5415);
#1514=VERTEX_POINT('',#5417);
#1515=VERTEX_POINT('',#5419);
#1516=VERTEX_POINT('',#5421);
#1517=VERTEX_POINT('',#5423);
#1518=VERTEX_POINT('',#5427);
#1519=VERTEX_POINT('',#5428);
#1520=VERTEX_POINT('',#5431);
#1521=VERTEX_POINT('',#5435);
#1522=VERTEX_POINT('',#5436);
#1523=VERTEX_POINT('',#5438);
#1524=VERTEX_POINT('',#5443);
#1525=VERTEX_POINT('',#5447);
#1526=VERTEX_POINT('',#5451);
#1527=VERTEX_POINT('',#5455);
#1528=VERTEX_POINT('',#5456);
#1529=VERTEX_POINT('',#5458);
#1530=VERTEX_POINT('',#5460);
#1531=VERTEX_POINT('',#5462);
#1532=VERTEX_POINT('',#5464);
#1533=VERTEX_POINT('',#5470);
#1534=VERTEX_POINT('',#5473);
#1535=VERTEX_POINT('',#5478);
#1536=VERTEX_POINT('',#5483);
#1537=VERTEX_POINT('',#5488);
#1538=VERTEX_POINT('',#5493);
#1539=VERTEX_POINT('',#5507);
#1540=VERTEX_POINT('',#5509);
#1541=VERTEX_POINT('',#5513);
#1542=VERTEX_POINT('',#5515);
#1543=VERTEX_POINT('',#5522);
#1544=VERTEX_POINT('',#5523);
#1545=VERTEX_POINT('',#5525);
#1546=VERTEX_POINT('',#5527);
#1547=VERTEX_POINT('',#5529);
#1548=VERTEX_POINT('',#5531);
#1549=VERTEX_POINT('',#5533);
#1550=VERTEX_POINT('',#5537);
#1551=VERTEX_POINT('',#5538);
#1552=VERTEX_POINT('',#5541);
#1553=VERTEX_POINT('',#5545);
#1554=VERTEX_POINT('',#5547);
#1555=VERTEX_POINT('',#5553);
#1556=VERTEX_POINT('',#5554);
#1557=VERTEX_POINT('',#5557);
#1558=VERTEX_POINT('',#5561);
#1559=VERTEX_POINT('',#5565);
#1560=VERTEX_POINT('',#5566);
#1561=VERTEX_POINT('',#5568);
#1562=VERTEX_POINT('',#5570);
#1563=VERTEX_POINT('',#5572);
#1564=VERTEX_POINT('',#5574);
#1565=VERTEX_POINT('',#5580);
#1566=VERTEX_POINT('',#5583);
#1567=VERTEX_POINT('',#5588);
#1568=VERTEX_POINT('',#5593);
#1569=VERTEX_POINT('',#5598);
#1570=VERTEX_POINT('',#5603);
#1571=EDGE_CURVE('',#1314,#1315,#1159,.T.);
#1572=EDGE_CURVE('',#1315,#1316,#767,.T.);
#1573=EDGE_CURVE('',#1316,#1317,#1160,.T.);
#1574=EDGE_CURVE('',#1317,#1314,#768,.T.);
#1575=EDGE_CURVE('',#1318,#1319,#769,.T.);
#1576=EDGE_CURVE('',#1320,#1318,#1161,.T.);
#1577=EDGE_CURVE('',#1321,#1320,#770,.T.);
#1578=EDGE_CURVE('',#1319,#1321,#1162,.T.);
#1579=EDGE_CURVE('',#1322,#1323,#1163,.T.);
#1580=EDGE_CURVE('',#1324,#1322,#771,.T.);
#1581=EDGE_CURVE('',#1325,#1324,#1164,.T.);
#1582=EDGE_CURVE('',#1323,#1325,#772,.T.);
#1583=EDGE_CURVE('',#1326,#1327,#1165,.T.);
#1584=EDGE_CURVE('',#1327,#1328,#773,.T.);
#1585=EDGE_CURVE('',#1328,#1329,#1166,.T.);
#1586=EDGE_CURVE('',#1329,#1326,#774,.T.);
#1587=EDGE_CURVE('',#1315,#1323,#775,.T.);
#1588=EDGE_CURVE('',#1314,#1322,#776,.T.);
#1589=EDGE_CURVE('',#1316,#1325,#777,.T.);
#1590=EDGE_CURVE('',#1317,#1324,#778,.T.);
#1591=EDGE_CURVE('',#1320,#1326,#779,.T.);
#1592=EDGE_CURVE('',#1318,#1327,#780,.T.);
#1593=EDGE_CURVE('',#1319,#1328,#781,.T.);
#1594=EDGE_CURVE('',#1321,#1329,#782,.T.);
#1595=EDGE_CURVE('',#1330,#1330,#1167,.T.);
#1596=EDGE_CURVE('',#1330,#1331,#783,.T.);
#1597=EDGE_CURVE('',#1331,#1331,#1168,.T.);
#1598=EDGE_CURVE('',#1332,#1332,#1169,.T.);
#1599=EDGE_CURVE('',#1332,#1333,#784,.T.);
#1600=EDGE_CURVE('',#1333,#1333,#1170,.T.);
#1601=EDGE_CURVE('',#1334,#1334,#1171,.T.);
#1602=EDGE_CURVE('',#1334,#1335,#785,.T.);
#1603=EDGE_CURVE('',#1335,#1335,#1172,.T.);
#1604=EDGE_CURVE('',#1336,#1336,#1173,.T.);
#1605=EDGE_CURVE('',#1336,#1337,#786,.T.);
#1606=EDGE_CURVE('',#1337,#1337,#1174,.T.);
#1607=EDGE_CURVE('',#1338,#1338,#1175,.T.);
#1608=EDGE_CURVE('',#1338,#1339,#787,.T.);
#1609=EDGE_CURVE('',#1339,#1339,#1176,.T.);
#1610=EDGE_CURVE('',#1340,#1340,#1177,.T.);
#1611=EDGE_CURVE('',#1340,#1341,#788,.T.);
#1612=EDGE_CURVE('',#1341,#1341,#1178,.T.);
#1613=EDGE_CURVE('',#1342,#1343,#789,.T.);
#1614=EDGE_CURVE('',#1343,#1344,#790,.T.);
#1615=EDGE_CURVE('',#1344,#1345,#1179,.T.);
#1616=EDGE_CURVE('',#1345,#1342,#791,.T.);
#1617=EDGE_CURVE('',#1346,#1347,#792,.T.);
#1618=EDGE_CURVE('',#1348,#1346,#793,.T.);
#1619=EDGE_CURVE('',#1349,#1348,#1180,.T.);
#1620=EDGE_CURVE('',#1347,#1349,#794,.T.);
#1621=EDGE_CURVE('',#1343,#1347,#795,.T.);
#1622=EDGE_CURVE('',#1342,#1346,#796,.T.);
#1623=EDGE_CURVE('',#1344,#1349,#797,.T.);
#1624=EDGE_CURVE('',#1345,#1348,#798,.T.);
#1625=EDGE_CURVE('',#1350,#1350,#1181,.T.);
#1626=EDGE_CURVE('',#1350,#1351,#1182,.T.);
#1627=EDGE_CURVE('',#1351,#1351,#1183,.T.);
#1628=EDGE_CURVE('',#1352,#1352,#1184,.T.);
#1629=EDGE_CURVE('',#1352,#1353,#1185,.T.);
#1630=EDGE_CURVE('',#1353,#1353,#1186,.T.);
#1631=EDGE_CURVE('',#1354,#1354,#166,.T.);
#1632=EDGE_CURVE('',#1354,#1355,#799,.T.);
#1633=EDGE_CURVE('',#1355,#1356,#167,.T.);
#1634=EDGE_CURVE('',#1356,#1355,#168,.T.);
#1635=EDGE_CURVE('',#1357,#1358,#169,.T.);
#1636=EDGE_CURVE('',#1358,#1359,#800,.T.);
#1637=EDGE_CURVE('',#1359,#1359,#170,.T.);
#1638=EDGE_CURVE('',#1358,#1357,#171,.T.);
#1639=EDGE_CURVE('',#1360,#1360,#1187,.T.);
#1640=EDGE_CURVE('',#1360,#1361,#801,.T.);
#1641=EDGE_CURVE('',#1361,#1361,#1188,.T.);
#1642=EDGE_CURVE('',#1362,#1362,#1189,.T.);
#1643=EDGE_CURVE('',#1362,#1363,#802,.T.);
#1644=EDGE_CURVE('',#1363,#1363,#1190,.T.);
#1645=EDGE_CURVE('',#1364,#1364,#1191,.T.);
#1646=EDGE_CURVE('',#1364,#1365,#803,.T.);
#1647=EDGE_CURVE('',#1365,#1365,#1192,.T.);
#1648=EDGE_CURVE('',#1366,#1366,#1193,.T.);
#1649=EDGE_CURVE('',#1366,#1367,#804,.T.);
#1650=EDGE_CURVE('',#1367,#1367,#1194,.T.);
#1651=EDGE_CURVE('',#1368,#1368,#1195,.T.);
#1652=EDGE_CURVE('',#1368,#1369,#805,.T.);
#1653=EDGE_CURVE('',#1369,#1369,#1196,.T.);
#1654=EDGE_CURVE('',#1351,#1370,#806,.T.);
#1655=EDGE_CURVE('',#1370,#1370,#1197,.T.);
#1656=EDGE_CURVE('',#1371,#1371,#1198,.T.);
#1657=EDGE_CURVE('',#1371,#1350,#807,.T.);
#1658=EDGE_CURVE('',#1372,#1372,#1199,.T.);
#1659=EDGE_CURVE('',#1372,#1352,#808,.T.);
#1660=EDGE_CURVE('',#1353,#1373,#809,.T.);
#1661=EDGE_CURVE('',#1373,#1373,#1200,.T.);
#1662=EDGE_CURVE('',#1374,#1374,#1201,.T.);
#1663=EDGE_CURVE('',#1374,#1375,#810,.T.);
#1664=EDGE_CURVE('',#1375,#1375,#1202,.T.);
#1665=EDGE_CURVE('',#1376,#1376,#1203,.T.);
#1666=EDGE_CURVE('',#1376,#1377,#811,.T.);
#1667=EDGE_CURVE('',#1377,#1377,#1204,.T.);
#1668=EDGE_CURVE('',#1378,#1378,#1205,.T.);
#1669=EDGE_CURVE('',#1378,#1379,#812,.T.);
#1670=EDGE_CURVE('',#1379,#1379,#1206,.T.);
#1671=EDGE_CURVE('',#1380,#1380,#1207,.T.);
#1672=EDGE_CURVE('',#1380,#1381,#1208,.T.);
#1673=EDGE_CURVE('',#1382,#1382,#1209,.T.);
#1674=EDGE_CURVE('',#1382,#1380,#813,.T.);
#1675=EDGE_CURVE('',#1383,#1384,#1210,.T.);
#1676=EDGE_CURVE('',#1383,#1385,#814,.T.);
#1677=EDGE_CURVE('',#1385,#1386,#1211,.T.);
#1678=EDGE_CURVE('',#1384,#1386,#815,.T.);
#1679=EDGE_CURVE('',#1384,#1387,#816,.T.);
#1680=EDGE_CURVE('',#1386,#1388,#817,.T.);
#1681=EDGE_CURVE('',#1387,#1388,#818,.T.);
#1682=EDGE_CURVE('',#1389,#1383,#819,.T.);
#1683=EDGE_CURVE('',#1389,#1390,#820,.T.);
#1684=EDGE_CURVE('',#1390,#1385,#821,.T.);
#1685=EDGE_CURVE('',#1391,#1392,#1212,.T.);
#1686=EDGE_CURVE('',#1393,#1391,#822,.T.);
#1687=EDGE_CURVE('',#1393,#1394,#1213,.T.);
#1688=EDGE_CURVE('',#1394,#1392,#823,.T.);
#1689=EDGE_CURVE('',#1395,#1391,#824,.T.);
#1690=EDGE_CURVE('',#1396,#1395,#825,.T.);
#1691=EDGE_CURVE('',#1396,#1393,#826,.T.);
#1692=EDGE_CURVE('',#1397,#1395,#1214,.T.);
#1693=EDGE_CURVE('',#1398,#1397,#827,.T.);
#1694=EDGE_CURVE('',#1398,#1396,#1215,.T.);
#1695=EDGE_CURVE('',#1399,#1397,#828,.T.);
#1696=EDGE_CURVE('',#1400,#1399,#829,.T.);
#1697=EDGE_CURVE('',#1400,#1398,#830,.T.);
#1698=EDGE_CURVE('',#1401,#1399,#1216,.T.);
#1699=EDGE_CURVE('',#1402,#1401,#831,.T.);
#1700=EDGE_CURVE('',#1402,#1400,#1217,.T.);
#1701=EDGE_CURVE('',#1403,#1401,#832,.T.);
#1702=EDGE_CURVE('',#1404,#1403,#833,.T.);
#1703=EDGE_CURVE('',#1404,#1402,#834,.T.);
#1704=EDGE_CURVE('',#1405,#1403,#1218,.T.);
#1705=EDGE_CURVE('',#1406,#1405,#835,.T.);
#1706=EDGE_CURVE('',#1406,#1404,#1219,.T.);
#1707=EDGE_CURVE('',#1392,#1405,#836,.T.);
#1708=EDGE_CURVE('',#1394,#1406,#837,.T.);
#1709=EDGE_CURVE('',#1407,#1408,#838,.T.);
#1710=EDGE_CURVE('',#1408,#1409,#839,.T.);
#1711=EDGE_CURVE('',#1410,#1409,#840,.T.);
#1712=EDGE_CURVE('',#1407,#1410,#841,.T.);
#1713=EDGE_CURVE('',#1387,#1389,#842,.T.);
#1714=EDGE_CURVE('',#1388,#1390,#843,.T.);
#1715=EDGE_CURVE('',#1411,#1412,#844,.T.);
#1716=EDGE_CURVE('',#1412,#1413,#1220,.T.);
#1717=EDGE_CURVE('',#1414,#1413,#845,.T.);
#1718=EDGE_CURVE('',#1411,#1414,#1221,.T.);
#1719=EDGE_CURVE('',#1413,#1408,#846,.T.);
#1720=EDGE_CURVE('',#1414,#1407,#847,.T.);
#1721=EDGE_CURVE('',#1409,#1412,#848,.T.);
#1722=EDGE_CURVE('',#1410,#1411,#849,.T.);
#1723=EDGE_CURVE('',#1415,#1415,#1222,.T.);
#1724=EDGE_CURVE('',#1415,#1416,#850,.T.);
#1725=EDGE_CURVE('',#1416,#1416,#1223,.T.);
#1726=EDGE_CURVE('',#1417,#1418,#851,.T.);
#1727=EDGE_CURVE('',#1418,#1419,#117,.T.);
#1728=EDGE_CURVE('',#1419,#1420,#118,.T.);
#1729=EDGE_CURVE('',#1421,#1420,#852,.T.);
#1730=EDGE_CURVE('',#1422,#1421,#119,.T.);
#1731=EDGE_CURVE('',#1417,#1422,#120,.T.);
#1732=EDGE_CURVE('',#1420,#1423,#121,.T.);
#1733=EDGE_CURVE('',#1423,#1424,#122,.T.);
#1734=EDGE_CURVE('',#1425,#1424,#853,.T.);
#1735=EDGE_CURVE('',#1426,#1425,#123,.T.);
#1736=EDGE_CURVE('',#1421,#1426,#124,.T.);
#1737=EDGE_CURVE('',#1427,#1428,#125,.T.);
#1738=EDGE_CURVE('',#1429,#1427,#854,.T.);
#1739=EDGE_CURVE('',#1429,#1430,#126,.T.);
#1740=EDGE_CURVE('',#1430,#1425,#127,.T.);
#1741=EDGE_CURVE('',#1428,#1424,#128,.T.);
#1742=EDGE_CURVE('',#1427,#1431,#129,.T.);
#1743=EDGE_CURVE('',#1431,#1432,#130,.T.);
#1744=EDGE_CURVE('',#1433,#1432,#855,.T.);
#1745=EDGE_CURVE('',#1434,#1433,#131,.T.);
#1746=EDGE_CURVE('',#1429,#1434,#132,.T.);
#1747=EDGE_CURVE('',#1432,#1435,#133,.T.);
#1748=EDGE_CURVE('',#1435,#1436,#134,.T.);
#1749=EDGE_CURVE('',#1437,#1436,#856,.T.);
#1750=EDGE_CURVE('',#1438,#1437,#135,.T.);
#1751=EDGE_CURVE('',#1433,#1438,#136,.T.);
#1752=EDGE_CURVE('',#1436,#1439,#137,.T.);
#1753=EDGE_CURVE('',#1439,#1418,#138,.T.);
#1754=EDGE_CURVE('',#1440,#1417,#139,.T.);
#1755=EDGE_CURVE('',#1437,#1440,#140,.T.);
#1756=EDGE_CURVE('',#1439,#1419,#1224,.T.);
#1757=EDGE_CURVE('',#1435,#1439,#1225,.T.);
#1758=EDGE_CURVE('',#1431,#1435,#1226,.T.);
#1759=EDGE_CURVE('',#1428,#1431,#1227,.T.);
#1760=EDGE_CURVE('',#1428,#1423,#1228,.T.);
#1761=EDGE_CURVE('',#1419,#1423,#1229,.T.);
#1762=EDGE_CURVE('',#1440,#1438,#1230,.T.);
#1763=EDGE_CURVE('',#1422,#1440,#1231,.T.);
#1764=EDGE_CURVE('',#1426,#1422,#1232,.T.);
#1765=EDGE_CURVE('',#1430,#1426,#1233,.T.);
#1766=EDGE_CURVE('',#1434,#1430,#1234,.T.);
#1767=EDGE_CURVE('',#1438,#1434,#1235,.T.);
#1768=EDGE_CURVE('',#1441,#1441,#1236,.T.);
#1769=EDGE_CURVE('',#1441,#1442,#857,.T.);
#1770=EDGE_CURVE('',#1442,#1442,#1237,.T.);
#1771=EDGE_CURVE('',#1443,#1444,#858,.T.);
#1772=EDGE_CURVE('',#1444,#1445,#141,.T.);
#1773=EDGE_CURVE('',#1445,#1446,#142,.T.);
#1774=EDGE_CURVE('',#1447,#1446,#859,.T.);
#1775=EDGE_CURVE('',#1448,#1447,#143,.T.);
#1776=EDGE_CURVE('',#1443,#1448,#144,.T.);
#1777=EDGE_CURVE('',#1446,#1449,#145,.T.);
#1778=EDGE_CURVE('',#1449,#1450,#146,.T.);
#1779=EDGE_CURVE('',#1451,#1450,#860,.T.);
#1780=EDGE_CURVE('',#1452,#1451,#147,.T.);
#1781=EDGE_CURVE('',#1447,#1452,#148,.T.);
#1782=EDGE_CURVE('',#1453,#1454,#149,.T.);
#1783=EDGE_CURVE('',#1455,#1453,#861,.T.);
#1784=EDGE_CURVE('',#1455,#1456,#150,.T.);
#1785=EDGE_CURVE('',#1456,#1451,#151,.T.);
#1786=EDGE_CURVE('',#1454,#1450,#152,.T.);
#1787=EDGE_CURVE('',#1453,#1457,#153,.T.);
#1788=EDGE_CURVE('',#1457,#1458,#154,.T.);
#1789=EDGE_CURVE('',#1459,#1458,#862,.T.);
#1790=EDGE_CURVE('',#1460,#1459,#155,.T.);
#1791=EDGE_CURVE('',#1455,#1460,#156,.T.);
#1792=EDGE_CURVE('',#1458,#1461,#157,.T.);
#1793=EDGE_CURVE('',#1461,#1462,#158,.T.);
#1794=EDGE_CURVE('',#1463,#1462,#863,.T.);
#1795=EDGE_CURVE('',#1464,#1463,#159,.T.);
#1796=EDGE_CURVE('',#1459,#1464,#160,.T.);
#1797=EDGE_CURVE('',#1462,#1465,#161,.T.);
#1798=EDGE_CURVE('',#1465,#1444,#162,.T.);
#1799=EDGE_CURVE('',#1466,#1443,#163,.T.);
#1800=EDGE_CURVE('',#1463,#1466,#164,.T.);
#1801=EDGE_CURVE('',#1465,#1445,#1238,.T.);
#1802=EDGE_CURVE('',#1461,#1465,#1239,.T.);
#1803=EDGE_CURVE('',#1457,#1461,#1240,.T.);
#1804=EDGE_CURVE('',#1454,#1457,#1241,.T.);
#1805=EDGE_CURVE('',#1454,#1449,#1242,.T.);
#1806=EDGE_CURVE('',#1445,#1449,#1243,.T.);
#1807=EDGE_CURVE('',#1466,#1464,#1244,.T.);
#1808=EDGE_CURVE('',#1448,#1466,#1245,.T.);
#1809=EDGE_CURVE('',#1452,#1448,#1246,.T.);
#1810=EDGE_CURVE('',#1456,#1452,#1247,.T.);
#1811=EDGE_CURVE('',#1460,#1456,#1248,.T.);
#1812=EDGE_CURVE('',#1464,#1460,#1249,.T.);
#1813=EDGE_CURVE('',#1467,#1467,#1250,.T.);
#1814=EDGE_CURVE('',#1467,#1468,#864,.T.);
#1815=EDGE_CURVE('',#1468,#1468,#1251,.T.);
#1816=EDGE_CURVE('',#1469,#1469,#1252,.T.);
#1817=EDGE_CURVE('',#1469,#1470,#865,.T.);
#1818=EDGE_CURVE('',#1470,#1470,#1253,.T.);
#1819=EDGE_CURVE('',#1471,#1471,#1254,.T.);
#1820=EDGE_CURVE('',#1471,#1472,#866,.T.);
#1821=EDGE_CURVE('',#1472,#1472,#1255,.T.);
#1822=EDGE_CURVE('',#1473,#1473,#1256,.T.);
#1823=EDGE_CURVE('',#1473,#1474,#867,.T.);
#1824=EDGE_CURVE('',#1474,#1474,#1257,.T.);
#1825=EDGE_CURVE('',#1475,#1475,#1258,.T.);
#1826=EDGE_CURVE('',#1475,#1476,#868,.T.);
#1827=EDGE_CURVE('',#1476,#1476,#1259,.T.);
#1828=EDGE_CURVE('',#1477,#1477,#1260,.T.);
#1829=EDGE_CURVE('',#1477,#1478,#869,.T.);
#1830=EDGE_CURVE('',#1478,#1478,#1261,.T.);
#1831=EDGE_CURVE('',#1479,#1479,#1262,.T.);
#1832=EDGE_CURVE('',#1479,#1480,#870,.T.);
#1833=EDGE_CURVE('',#1480,#1480,#1263,.T.);
#1834=EDGE_CURVE('',#1481,#1481,#1264,.T.);
#1835=EDGE_CURVE('',#1481,#1482,#871,.T.);
#1836=EDGE_CURVE('',#1482,#1482,#1265,.T.);
#1837=EDGE_CURVE('',#1483,#1484,#872,.T.);
#1838=EDGE_CURVE('',#1484,#1485,#873,.T.);
#1839=EDGE_CURVE('',#1486,#1485,#874,.T.);
#1840=EDGE_CURVE('',#1483,#1486,#875,.T.);
#1841=EDGE_CURVE('',#1487,#1488,#876,.T.);
#1842=EDGE_CURVE('',#1489,#1487,#877,.T.);
#1843=EDGE_CURVE('',#1489,#1490,#878,.T.);
#1844=EDGE_CURVE('',#1490,#1488,#879,.T.);
#1845=EDGE_CURVE('',#1491,#1492,#880,.T.);
#1846=EDGE_CURVE('',#1491,#1493,#881,.T.);
#1847=EDGE_CURVE('',#1493,#1494,#882,.T.);
#1848=EDGE_CURVE('',#1492,#1494,#883,.T.);
#1849=EDGE_CURVE('',#1495,#1496,#884,.T.);
#1850=EDGE_CURVE('',#1496,#1497,#885,.T.);
#1851=EDGE_CURVE('',#1498,#1497,#886,.T.);
#1852=EDGE_CURVE('',#1495,#1498,#887,.T.);
#1853=EDGE_CURVE('',#1484,#1492,#888,.T.);
#1854=EDGE_CURVE('',#1483,#1491,#889,.T.);
#1855=EDGE_CURVE('',#1485,#1494,#890,.T.);
#1856=EDGE_CURVE('',#1486,#1493,#891,.T.);
#1857=EDGE_CURVE('',#1489,#1495,#892,.T.);
#1858=EDGE_CURVE('',#1487,#1496,#893,.T.);
#1859=EDGE_CURVE('',#1488,#1497,#894,.T.);
#1860=EDGE_CURVE('',#1490,#1498,#895,.T.);
#1861=EDGE_CURVE('',#1499,#1500,#1266,.T.);
#1862=EDGE_CURVE('',#1500,#1499,#1267,.T.);
#1863=EDGE_CURVE('',#1500,#1501,#896,.T.);
#1864=EDGE_CURVE('',#1501,#1501,#1268,.T.);
#1865=EDGE_CURVE('',#1502,#1503,#1269,.T.);
#1866=EDGE_CURVE('',#1503,#1502,#1270,.T.);
#1867=EDGE_CURVE('',#1503,#1504,#897,.T.);
#1868=EDGE_CURVE('',#1504,#1504,#1271,.T.);
#1869=EDGE_CURVE('',#1505,#1505,#1272,.T.);
#1870=EDGE_CURVE('',#1505,#1506,#898,.T.);
#1871=EDGE_CURVE('',#1506,#1506,#1273,.T.);
#1872=EDGE_CURVE('',#1507,#1507,#1274,.T.);
#1873=EDGE_CURVE('',#1507,#1508,#899,.T.);
#1874=EDGE_CURVE('',#1508,#1508,#1275,.T.);
#1875=EDGE_CURVE('',#1499,#1507,#900,.T.);
#1876=EDGE_CURVE('',#1509,#1509,#1276,.T.);
#1877=EDGE_CURVE('',#1509,#1505,#901,.T.);
#1878=EDGE_CURVE('',#1502,#1510,#902,.T.);
#1879=EDGE_CURVE('',#1510,#1510,#1277,.T.);
#1880=EDGE_CURVE('',#1511,#1512,#903,.T.);
#1881=EDGE_CURVE('',#1512,#1513,#1278,.T.);
#1882=EDGE_CURVE('',#1513,#1514,#1279,.T.);
#1883=EDGE_CURVE('',#1514,#1515,#1280,.T.);
#1884=EDGE_CURVE('',#1515,#1516,#1281,.T.);
#1885=EDGE_CURVE('',#1516,#1517,#1282,.T.);
#1886=EDGE_CURVE('',#1517,#1512,#1283,.T.);
#1887=EDGE_CURVE('',#1518,#1519,#1284,.T.);
#1888=EDGE_CURVE('',#1519,#1518,#1285,.T.);
#1889=EDGE_CURVE('',#1519,#1520,#1286,.T.);
#1890=EDGE_CURVE('',#1520,#1520,#1287,.T.);
#1891=EDGE_CURVE('',#1521,#1522,#1288,.T.);
#1892=EDGE_CURVE('',#1522,#1523,#904,.T.);
#1893=EDGE_CURVE('',#1523,#1523,#1289,.T.);
#1894=EDGE_CURVE('',#1522,#1521,#1290,.T.);
#1895=EDGE_CURVE('',#1521,#1524,#905,.T.);
#1896=EDGE_CURVE('',#1524,#1524,#1291,.T.);
#1897=EDGE_CURVE('',#1518,#1525,#906,.T.);
#1898=EDGE_CURVE('',#1525,#1525,#1292,.T.);
#1899=EDGE_CURVE('',#1525,#1526,#907,.T.);
#1900=EDGE_CURVE('',#1526,#1526,#1293,.T.);
#1901=EDGE_CURVE('',#1527,#1528,#908,.T.);
#1902=EDGE_CURVE('',#1529,#1528,#909,.T.);
#1903=EDGE_CURVE('',#1529,#1530,#910,.T.);
#1904=EDGE_CURVE('',#1530,#1531,#911,.T.);
#1905=EDGE_CURVE('',#1532,#1531,#912,.T.);
#1906=EDGE_CURVE('',#1527,#1532,#913,.T.);
#1907=EDGE_CURVE('',#1533,#1527,#914,.T.);
#1908=EDGE_CURVE('',#1533,#1516,#915,.T.);
#1909=EDGE_CURVE('',#1516,#1534,#916,.T.);
#1910=EDGE_CURVE('',#1534,#1528,#917,.T.);
#1911=EDGE_CURVE('',#1515,#1534,#918,.T.);
#1912=EDGE_CURVE('',#1535,#1515,#919,.T.);
#1913=EDGE_CURVE('',#1535,#1529,#920,.T.);
#1914=EDGE_CURVE('',#1535,#1514,#921,.T.);
#1915=EDGE_CURVE('',#1514,#1536,#922,.T.);
#1916=EDGE_CURVE('',#1536,#1530,#923,.T.);
#1917=EDGE_CURVE('',#1536,#1513,#924,.T.);
#1918=EDGE_CURVE('',#1513,#1537,#925,.T.);
#1919=EDGE_CURVE('',#1537,#1531,#926,.T.);
#1920=EDGE_CURVE('',#1512,#1537,#927,.T.);
#1921=EDGE_CURVE('',#1538,#1512,#928,.T.);
#1922=EDGE_CURVE('',#1538,#1532,#929,.T.);
#1923=EDGE_CURVE('',#1517,#1538,#930,.T.);
#1924=EDGE_CURVE('',#1533,#1517,#931,.T.);
#1925=EDGE_CURVE('',#1539,#1539,#1294,.T.);
#1926=EDGE_CURVE('',#1539,#1540,#932,.T.);
#1927=EDGE_CURVE('',#1540,#1540,#1295,.T.);
#1928=EDGE_CURVE('',#1541,#1541,#1296,.T.);
#1929=EDGE_CURVE('',#1541,#1542,#933,.T.);
#1930=EDGE_CURVE('',#1542,#1542,#1297,.T.);
#1931=EDGE_CURVE('',#1543,#1544,#934,.T.);
#1932=EDGE_CURVE('',#1544,#1545,#1298,.T.);
#1933=EDGE_CURVE('',#1545,#1546,#1299,.T.);
#1934=EDGE_CURVE('',#1546,#1547,#1300,.T.);
#1935=EDGE_CURVE('',#1547,#1548,#1301,.T.);
#1936=EDGE_CURVE('',#1548,#1549,#1302,.T.);
#1937=EDGE_CURVE('',#1549,#1544,#1303,.T.);
#1938=EDGE_CURVE('',#1550,#1551,#1304,.T.);
#1939=EDGE_CURVE('',#1551,#1550,#1305,.T.);
#1940=EDGE_CURVE('',#1551,#1552,#1306,.T.);
#1941=EDGE_CURVE('',#1552,#1552,#1307,.T.);
#1942=EDGE_CURVE('',#1553,#1553,#1308,.T.);
#1943=EDGE_CURVE('',#1553,#1554,#935,.T.);
#1944=EDGE_CURVE('',#1554,#1554,#1309,.T.);
#1945=EDGE_CURVE('',#1550,#1553,#936,.T.);
#1946=EDGE_CURVE('',#1555,#1556,#1310,.T.);
#1947=EDGE_CURVE('',#1556,#1555,#1311,.T.);
#1948=EDGE_CURVE('',#1556,#1557,#937,.T.);
#1949=EDGE_CURVE('',#1557,#1557,#1312,.T.);
#1950=EDGE_CURVE('',#1555,#1558,#938,.T.);
#1951=EDGE_CURVE('',#1558,#1558,#1313,.T.);
#1952=EDGE_CURVE('',#1559,#1560,#939,.T.);
#1953=EDGE_CURVE('',#1561,#1560,#940,.T.);
#1954=EDGE_CURVE('',#1561,#1562,#941,.T.);
#1955=EDGE_CURVE('',#1562,#1563,#942,.T.);
#1956=EDGE_CURVE('',#1564,#1563,#943,.T.);
#1957=EDGE_CURVE('',#1559,#1564,#944,.T.);
#1958=EDGE_CURVE('',#1565,#1559,#945,.T.);
#1959=EDGE_CURVE('',#1565,#1548,#946,.T.);
#1960=EDGE_CURVE('',#1548,#1566,#947,.T.);
#1961=EDGE_CURVE('',#1566,#1560,#948,.T.);
#1962=EDGE_CURVE('',#1547,#1566,#949,.T.);
#1963=EDGE_CURVE('',#1567,#1547,#950,.T.);
#1964=EDGE_CURVE('',#1567,#1561,#951,.T.);
#1965=EDGE_CURVE('',#1567,#1546,#952,.T.);
#1966=EDGE_CURVE('',#1546,#1568,#953,.T.);
#1967=EDGE_CURVE('',#1568,#1562,#954,.T.);
#1968=EDGE_CURVE('',#1568,#1545,#955,.T.);
#1969=EDGE_CURVE('',#1545,#1569,#956,.T.);
#1970=EDGE_CURVE('',#1569,#1563,#957,.T.);
#1971=EDGE_CURVE('',#1544,#1569,#958,.T.);
#1972=EDGE_CURVE('',#1570,#1544,#959,.T.);
#1973=EDGE_CURVE('',#1570,#1564,#960,.T.);
#1974=EDGE_CURVE('',#1549,#1570,#961,.T.);
#1975=EDGE_CURVE('',#1565,#1549,#962,.T.);
#1976=ORIENTED_EDGE('',*,*,#1571,.T.);
#1977=ORIENTED_EDGE('',*,*,#1572,.T.);
#1978=ORIENTED_EDGE('',*,*,#1573,.T.);
#1979=ORIENTED_EDGE('',*,*,#1574,.T.);
#1980=ORIENTED_EDGE('',*,*,#1575,.F.);
#1981=ORIENTED_EDGE('',*,*,#1576,.F.);
#1982=ORIENTED_EDGE('',*,*,#1577,.F.);
#1983=ORIENTED_EDGE('',*,*,#1578,.F.);
#1984=ORIENTED_EDGE('',*,*,#1579,.F.);
#1985=ORIENTED_EDGE('',*,*,#1580,.F.);
#1986=ORIENTED_EDGE('',*,*,#1581,.F.);
#1987=ORIENTED_EDGE('',*,*,#1582,.F.);
#1988=ORIENTED_EDGE('',*,*,#1583,.T.);
#1989=ORIENTED_EDGE('',*,*,#1584,.T.);
#1990=ORIENTED_EDGE('',*,*,#1585,.T.);
#1991=ORIENTED_EDGE('',*,*,#1586,.T.);
#1992=ORIENTED_EDGE('',*,*,#1579,.T.);
#1993=ORIENTED_EDGE('',*,*,#1587,.F.);
#1994=ORIENTED_EDGE('',*,*,#1571,.F.);
#1995=ORIENTED_EDGE('',*,*,#1588,.T.);
#1996=ORIENTED_EDGE('',*,*,#1582,.T.);
#1997=ORIENTED_EDGE('',*,*,#1589,.F.);
#1998=ORIENTED_EDGE('',*,*,#1572,.F.);
#1999=ORIENTED_EDGE('',*,*,#1587,.T.);
#2000=ORIENTED_EDGE('',*,*,#1581,.T.);
#2001=ORIENTED_EDGE('',*,*,#1590,.F.);
#2002=ORIENTED_EDGE('',*,*,#1573,.F.);
#2003=ORIENTED_EDGE('',*,*,#1589,.T.);
#2004=ORIENTED_EDGE('',*,*,#1580,.T.);
#2005=ORIENTED_EDGE('',*,*,#1588,.F.);
#2006=ORIENTED_EDGE('',*,*,#1574,.F.);
#2007=ORIENTED_EDGE('',*,*,#1590,.T.);
#2008=ORIENTED_EDGE('',*,*,#1583,.F.);
#2009=ORIENTED_EDGE('',*,*,#1591,.F.);
#2010=ORIENTED_EDGE('',*,*,#1576,.T.);
#2011=ORIENTED_EDGE('',*,*,#1592,.T.);
#2012=ORIENTED_EDGE('',*,*,#1584,.F.);
#2013=ORIENTED_EDGE('',*,*,#1592,.F.);
#2014=ORIENTED_EDGE('',*,*,#1575,.T.);
#2015=ORIENTED_EDGE('',*,*,#1593,.T.);
#2016=ORIENTED_EDGE('',*,*,#1585,.F.);
#2017=ORIENTED_EDGE('',*,*,#1593,.F.);
#2018=ORIENTED_EDGE('',*,*,#1578,.T.);
#2019=ORIENTED_EDGE('',*,*,#1594,.T.);
#2020=ORIENTED_EDGE('',*,*,#1586,.F.);
#2021=ORIENTED_EDGE('',*,*,#1594,.F.);
#2022=ORIENTED_EDGE('',*,*,#1577,.T.);
#2023=ORIENTED_EDGE('',*,*,#1591,.T.);
#2024=ORIENTED_EDGE('',*,*,#1595,.T.);
#2025=ORIENTED_EDGE('',*,*,#1596,.T.);
#2026=ORIENTED_EDGE('',*,*,#1597,.F.);
#2027=ORIENTED_EDGE('',*,*,#1596,.F.);
#2028=ORIENTED_EDGE('',*,*,#1598,.T.);
#2029=ORIENTED_EDGE('',*,*,#1599,.T.);
#2030=ORIENTED_EDGE('',*,*,#1600,.F.);
#2031=ORIENTED_EDGE('',*,*,#1599,.F.);
#2032=ORIENTED_EDGE('',*,*,#1601,.T.);
#2033=ORIENTED_EDGE('',*,*,#1602,.T.);
#2034=ORIENTED_EDGE('',*,*,#1603,.F.);
#2035=ORIENTED_EDGE('',*,*,#1602,.F.);
#2036=ORIENTED_EDGE('',*,*,#1604,.T.);
#2037=ORIENTED_EDGE('',*,*,#1605,.T.);
#2038=ORIENTED_EDGE('',*,*,#1606,.F.);
#2039=ORIENTED_EDGE('',*,*,#1605,.F.);
#2040=ORIENTED_EDGE('',*,*,#1607,.T.);
#2041=ORIENTED_EDGE('',*,*,#1608,.T.);
#2042=ORIENTED_EDGE('',*,*,#1609,.F.);
#2043=ORIENTED_EDGE('',*,*,#1608,.F.);
#2044=ORIENTED_EDGE('',*,*,#1610,.T.);
#2045=ORIENTED_EDGE('',*,*,#1611,.T.);
#2046=ORIENTED_EDGE('',*,*,#1612,.F.);
#2047=ORIENTED_EDGE('',*,*,#1611,.F.);
#2048=ORIENTED_EDGE('',*,*,#1613,.T.);
#2049=ORIENTED_EDGE('',*,*,#1614,.T.);
#2050=ORIENTED_EDGE('',*,*,#1615,.T.);
#2051=ORIENTED_EDGE('',*,*,#1616,.T.);
#2052=ORIENTED_EDGE('',*,*,#1607,.F.);
#2053=ORIENTED_EDGE('',*,*,#1601,.F.);
#2054=ORIENTED_EDGE('',*,*,#1595,.F.);
#2055=ORIENTED_EDGE('',*,*,#1598,.F.);
#2056=ORIENTED_EDGE('',*,*,#1604,.F.);
#2057=ORIENTED_EDGE('',*,*,#1610,.F.);
#2058=ORIENTED_EDGE('',*,*,#1617,.F.);
#2059=ORIENTED_EDGE('',*,*,#1618,.F.);
#2060=ORIENTED_EDGE('',*,*,#1619,.F.);
#2061=ORIENTED_EDGE('',*,*,#1620,.F.);
#2062=ORIENTED_EDGE('',*,*,#1612,.T.);
#2063=ORIENTED_EDGE('',*,*,#1609,.T.);
#2064=ORIENTED_EDGE('',*,*,#1606,.T.);
#2065=ORIENTED_EDGE('',*,*,#1603,.T.);
#2066=ORIENTED_EDGE('',*,*,#1600,.T.);
#2067=ORIENTED_EDGE('',*,*,#1597,.T.);
#2068=ORIENTED_EDGE('',*,*,#1617,.T.);
#2069=ORIENTED_EDGE('',*,*,#1621,.F.);
#2070=ORIENTED_EDGE('',*,*,#1613,.F.);
#2071=ORIENTED_EDGE('',*,*,#1622,.T.);
#2072=ORIENTED_EDGE('',*,*,#1620,.T.);
#2073=ORIENTED_EDGE('',*,*,#1623,.F.);
#2074=ORIENTED_EDGE('',*,*,#1614,.F.);
#2075=ORIENTED_EDGE('',*,*,#1621,.T.);
#2076=ORIENTED_EDGE('',*,*,#1619,.T.);
#2077=ORIENTED_EDGE('',*,*,#1624,.F.);
#2078=ORIENTED_EDGE('',*,*,#1615,.F.);
#2079=ORIENTED_EDGE('',*,*,#1623,.T.);
#2080=ORIENTED_EDGE('',*,*,#1618,.T.);
#2081=ORIENTED_EDGE('',*,*,#1622,.F.);
#2082=ORIENTED_EDGE('',*,*,#1616,.F.);
#2083=ORIENTED_EDGE('',*,*,#1624,.T.);
#2084=ORIENTED_EDGE('',*,*,#1625,.T.);
#2085=ORIENTED_EDGE('',*,*,#1626,.T.);
#2086=ORIENTED_EDGE('',*,*,#1627,.F.);
#2087=ORIENTED_EDGE('',*,*,#1626,.F.);
#2088=ORIENTED_EDGE('',*,*,#1628,.T.);
#2089=ORIENTED_EDGE('',*,*,#1629,.T.);
#2090=ORIENTED_EDGE('',*,*,#1630,.F.);
#2091=ORIENTED_EDGE('',*,*,#1629,.F.);
#2092=ORIENTED_EDGE('',*,*,#1631,.F.);
#2093=ORIENTED_EDGE('',*,*,#1632,.T.);
#2094=ORIENTED_EDGE('',*,*,#1633,.T.);
#2095=ORIENTED_EDGE('',*,*,#1634,.T.);
#2096=ORIENTED_EDGE('',*,*,#1632,.F.);
#2097=ORIENTED_EDGE('',*,*,#1635,.T.);
#2098=ORIENTED_EDGE('',*,*,#1636,.T.);
#2099=ORIENTED_EDGE('',*,*,#1637,.F.);
#2100=ORIENTED_EDGE('',*,*,#1636,.F.);
#2101=ORIENTED_EDGE('',*,*,#1638,.T.);
#2102=ORIENTED_EDGE('',*,*,#1639,.T.);
#2103=ORIENTED_EDGE('',*,*,#1640,.T.);
#2104=ORIENTED_EDGE('',*,*,#1641,.F.);
#2105=ORIENTED_EDGE('',*,*,#1640,.F.);
#2106=ORIENTED_EDGE('',*,*,#1642,.T.);
#2107=ORIENTED_EDGE('',*,*,#1643,.T.);
#2108=ORIENTED_EDGE('',*,*,#1644,.F.);
#2109=ORIENTED_EDGE('',*,*,#1643,.F.);
#2110=ORIENTED_EDGE('',*,*,#1645,.T.);
#2111=ORIENTED_EDGE('',*,*,#1646,.T.);
#2112=ORIENTED_EDGE('',*,*,#1647,.F.);
#2113=ORIENTED_EDGE('',*,*,#1646,.F.);
#2114=ORIENTED_EDGE('',*,*,#1648,.T.);
#2115=ORIENTED_EDGE('',*,*,#1649,.T.);
#2116=ORIENTED_EDGE('',*,*,#1650,.F.);
#2117=ORIENTED_EDGE('',*,*,#1649,.F.);
#2118=ORIENTED_EDGE('',*,*,#1651,.T.);
#2119=ORIENTED_EDGE('',*,*,#1652,.T.);
#2120=ORIENTED_EDGE('',*,*,#1653,.F.);
#2121=ORIENTED_EDGE('',*,*,#1652,.F.);
#2122=ORIENTED_EDGE('',*,*,#1627,.T.);
#2123=ORIENTED_EDGE('',*,*,#1654,.T.);
#2124=ORIENTED_EDGE('',*,*,#1655,.F.);
#2125=ORIENTED_EDGE('',*,*,#1654,.F.);
#2126=ORIENTED_EDGE('',*,*,#1656,.T.);
#2127=ORIENTED_EDGE('',*,*,#1657,.T.);
#2128=ORIENTED_EDGE('',*,*,#1625,.F.);
#2129=ORIENTED_EDGE('',*,*,#1657,.F.);
#2130=ORIENTED_EDGE('',*,*,#1635,.F.);
#2131=ORIENTED_EDGE('',*,*,#1638,.F.);
#2132=ORIENTED_EDGE('',*,*,#1634,.F.);
#2133=ORIENTED_EDGE('',*,*,#1633,.F.);
#2134=ORIENTED_EDGE('',*,*,#1658,.T.);
#2135=ORIENTED_EDGE('',*,*,#1659,.T.);
#2136=ORIENTED_EDGE('',*,*,#1628,.F.);
#2137=ORIENTED_EDGE('',*,*,#1659,.F.);
#2138=ORIENTED_EDGE('',*,*,#1630,.T.);
#2139=ORIENTED_EDGE('',*,*,#1660,.T.);
#2140=ORIENTED_EDGE('',*,*,#1661,.F.);
#2141=ORIENTED_EDGE('',*,*,#1660,.F.);
#2142=ORIENTED_EDGE('',*,*,#1631,.T.);
#2143=ORIENTED_EDGE('',*,*,#1637,.T.);
#2144=ORIENTED_EDGE('',*,*,#1661,.T.);
#2145=ORIENTED_EDGE('',*,*,#1656,.F.);
#2146=ORIENTED_EDGE('',*,*,#1655,.T.);
#2147=ORIENTED_EDGE('',*,*,#1653,.T.);
#2148=ORIENTED_EDGE('',*,*,#1645,.F.);
#2149=ORIENTED_EDGE('',*,*,#1639,.F.);
#2150=ORIENTED_EDGE('',*,*,#1658,.F.);
#2151=ORIENTED_EDGE('',*,*,#1642,.F.);
#2152=ORIENTED_EDGE('',*,*,#1648,.F.);
#2153=ORIENTED_EDGE('',*,*,#1651,.F.);
#2154=ORIENTED_EDGE('',*,*,#1650,.T.);
#2155=ORIENTED_EDGE('',*,*,#1647,.T.);
#2156=ORIENTED_EDGE('',*,*,#1644,.T.);
#2157=ORIENTED_EDGE('',*,*,#1641,.T.);
#2158=ORIENTED_EDGE('',*,*,#1662,.F.);
#2159=ORIENTED_EDGE('',*,*,#1663,.T.);
#2160=ORIENTED_EDGE('',*,*,#1664,.T.);
#2161=ORIENTED_EDGE('',*,*,#1663,.F.);
#2162=ORIENTED_EDGE('',*,*,#1665,.F.);
#2163=ORIENTED_EDGE('',*,*,#1666,.T.);
#2164=ORIENTED_EDGE('',*,*,#1667,.T.);
#2165=ORIENTED_EDGE('',*,*,#1666,.F.);
#2166=ORIENTED_EDGE('',*,*,#1668,.F.);
#2167=ORIENTED_EDGE('',*,*,#1669,.T.);
#2168=ORIENTED_EDGE('',*,*,#1670,.T.);
#2169=ORIENTED_EDGE('',*,*,#1669,.F.);
#2170=ORIENTED_EDGE('',*,*,#1671,.F.);
#2171=ORIENTED_EDGE('',*,*,#1672,.T.);
#2172=ORIENTED_EDGE('',*,*,#1672,.F.);
#2173=ORIENTED_EDGE('',*,*,#1673,.F.);
#2174=ORIENTED_EDGE('',*,*,#1674,.T.);
#2175=ORIENTED_EDGE('',*,*,#1671,.T.);
#2176=ORIENTED_EDGE('',*,*,#1674,.F.);
#2177=ORIENTED_EDGE('',*,*,#1675,.F.);
#2178=ORIENTED_EDGE('',*,*,#1676,.T.);
#2179=ORIENTED_EDGE('',*,*,#1677,.T.);
#2180=ORIENTED_EDGE('',*,*,#1678,.F.);
#2181=ORIENTED_EDGE('',*,*,#1679,.F.);
#2182=ORIENTED_EDGE('',*,*,#1678,.T.);
#2183=ORIENTED_EDGE('',*,*,#1680,.T.);
#2184=ORIENTED_EDGE('',*,*,#1681,.F.);
#2185=ORIENTED_EDGE('',*,*,#1682,.F.);
#2186=ORIENTED_EDGE('',*,*,#1683,.T.);
#2187=ORIENTED_EDGE('',*,*,#1684,.T.);
#2188=ORIENTED_EDGE('',*,*,#1676,.F.);
#2189=ORIENTED_EDGE('',*,*,#1685,.F.);
#2190=ORIENTED_EDGE('',*,*,#1686,.F.);
#2191=ORIENTED_EDGE('',*,*,#1687,.T.);
#2192=ORIENTED_EDGE('',*,*,#1688,.T.);
#2193=ORIENTED_EDGE('',*,*,#1689,.F.);
#2194=ORIENTED_EDGE('',*,*,#1690,.F.);
#2195=ORIENTED_EDGE('',*,*,#1691,.T.);
#2196=ORIENTED_EDGE('',*,*,#1686,.T.);
#2197=ORIENTED_EDGE('',*,*,#1692,.F.);
#2198=ORIENTED_EDGE('',*,*,#1693,.F.);
#2199=ORIENTED_EDGE('',*,*,#1694,.T.);
#2200=ORIENTED_EDGE('',*,*,#1690,.T.);
#2201=ORIENTED_EDGE('',*,*,#1695,.F.);
#2202=ORIENTED_EDGE('',*,*,#1696,.F.);
#2203=ORIENTED_EDGE('',*,*,#1697,.T.);
#2204=ORIENTED_EDGE('',*,*,#1693,.T.);
#2205=ORIENTED_EDGE('',*,*,#1698,.F.);
#2206=ORIENTED_EDGE('',*,*,#1699,.F.);
#2207=ORIENTED_EDGE('',*,*,#1700,.T.);
#2208=ORIENTED_EDGE('',*,*,#1696,.T.);
#2209=ORIENTED_EDGE('',*,*,#1701,.F.);
#2210=ORIENTED_EDGE('',*,*,#1702,.F.);
#2211=ORIENTED_EDGE('',*,*,#1703,.T.);
#2212=ORIENTED_EDGE('',*,*,#1699,.T.);
#2213=ORIENTED_EDGE('',*,*,#1704,.F.);
#2214=ORIENTED_EDGE('',*,*,#1705,.F.);
#2215=ORIENTED_EDGE('',*,*,#1706,.T.);
#2216=ORIENTED_EDGE('',*,*,#1702,.T.);
#2217=ORIENTED_EDGE('',*,*,#1707,.F.);
#2218=ORIENTED_EDGE('',*,*,#1688,.F.);
#2219=ORIENTED_EDGE('',*,*,#1708,.T.);
#2220=ORIENTED_EDGE('',*,*,#1705,.T.);
#2221=ORIENTED_EDGE('',*,*,#1687,.F.);
#2222=ORIENTED_EDGE('',*,*,#1691,.F.);
#2223=ORIENTED_EDGE('',*,*,#1694,.F.);
#2224=ORIENTED_EDGE('',*,*,#1697,.F.);
#2225=ORIENTED_EDGE('',*,*,#1700,.F.);
#2226=ORIENTED_EDGE('',*,*,#1703,.F.);
#2227=ORIENTED_EDGE('',*,*,#1706,.F.);
#2228=ORIENTED_EDGE('',*,*,#1708,.F.);
#2229=ORIENTED_EDGE('',*,*,#1709,.T.);
#2230=ORIENTED_EDGE('',*,*,#1710,.T.);
#2231=ORIENTED_EDGE('',*,*,#1711,.F.);
#2232=ORIENTED_EDGE('',*,*,#1712,.F.);
#2233=ORIENTED_EDGE('',*,*,#1713,.F.);
#2234=ORIENTED_EDGE('',*,*,#1681,.T.);
#2235=ORIENTED_EDGE('',*,*,#1714,.T.);
#2236=ORIENTED_EDGE('',*,*,#1683,.F.);
#2237=ORIENTED_EDGE('',*,*,#1685,.T.);
#2238=ORIENTED_EDGE('',*,*,#1707,.T.);
#2239=ORIENTED_EDGE('',*,*,#1704,.T.);
#2240=ORIENTED_EDGE('',*,*,#1701,.T.);
#2241=ORIENTED_EDGE('',*,*,#1698,.T.);
#2242=ORIENTED_EDGE('',*,*,#1695,.T.);
#2243=ORIENTED_EDGE('',*,*,#1692,.T.);
#2244=ORIENTED_EDGE('',*,*,#1689,.T.);
#2245=ORIENTED_EDGE('',*,*,#1668,.T.);
#2246=ORIENTED_EDGE('',*,*,#1670,.F.);
#2247=ORIENTED_EDGE('',*,*,#1673,.T.);
#2248=ORIENTED_EDGE('',*,*,#1715,.T.);
#2249=ORIENTED_EDGE('',*,*,#1716,.T.);
#2250=ORIENTED_EDGE('',*,*,#1717,.F.);
#2251=ORIENTED_EDGE('',*,*,#1718,.F.);
#2252=ORIENTED_EDGE('',*,*,#1717,.T.);
#2253=ORIENTED_EDGE('',*,*,#1719,.T.);
#2254=ORIENTED_EDGE('',*,*,#1709,.F.);
#2255=ORIENTED_EDGE('',*,*,#1720,.F.);
#2256=ORIENTED_EDGE('',*,*,#1711,.T.);
#2257=ORIENTED_EDGE('',*,*,#1721,.T.);
#2258=ORIENTED_EDGE('',*,*,#1715,.F.);
#2259=ORIENTED_EDGE('',*,*,#1722,.F.);
#2260=ORIENTED_EDGE('',*,*,#1718,.T.);
#2261=ORIENTED_EDGE('',*,*,#1720,.T.);
#2262=ORIENTED_EDGE('',*,*,#1712,.T.);
#2263=ORIENTED_EDGE('',*,*,#1722,.T.);
#2264=ORIENTED_EDGE('',*,*,#1667,.F.);
#2265=ORIENTED_EDGE('',*,*,#1677,.F.);
#2266=ORIENTED_EDGE('',*,*,#1684,.F.);
#2267=ORIENTED_EDGE('',*,*,#1714,.F.);
#2268=ORIENTED_EDGE('',*,*,#1680,.F.);
#2269=ORIENTED_EDGE('',*,*,#1662,.T.);
#2270=ORIENTED_EDGE('',*,*,#1675,.T.);
#2271=ORIENTED_EDGE('',*,*,#1679,.T.);
#2272=ORIENTED_EDGE('',*,*,#1713,.T.);
#2273=ORIENTED_EDGE('',*,*,#1682,.T.);
#2274=ORIENTED_EDGE('',*,*,#1664,.F.);
#2275=ORIENTED_EDGE('',*,*,#1716,.F.);
#2276=ORIENTED_EDGE('',*,*,#1721,.F.);
#2277=ORIENTED_EDGE('',*,*,#1710,.F.);
#2278=ORIENTED_EDGE('',*,*,#1719,.F.);
#2279=ORIENTED_EDGE('',*,*,#1665,.T.);
#2280=ORIENTED_EDGE('',*,*,#1723,.F.);
#2281=ORIENTED_EDGE('',*,*,#1724,.T.);
#2282=ORIENTED_EDGE('',*,*,#1725,.T.);
#2283=ORIENTED_EDGE('',*,*,#1724,.F.);
#2284=ORIENTED_EDGE('',*,*,#1726,.T.);
#2285=ORIENTED_EDGE('',*,*,#1727,.T.);
#2286=ORIENTED_EDGE('',*,*,#1728,.T.);
#2287=ORIENTED_EDGE('',*,*,#1729,.F.);
#2288=ORIENTED_EDGE('',*,*,#1730,.F.);
#2289=ORIENTED_EDGE('',*,*,#1731,.F.);
#2290=ORIENTED_EDGE('',*,*,#1729,.T.);
#2291=ORIENTED_EDGE('',*,*,#1732,.T.);
#2292=ORIENTED_EDGE('',*,*,#1733,.T.);
#2293=ORIENTED_EDGE('',*,*,#1734,.F.);
#2294=ORIENTED_EDGE('',*,*,#1735,.F.);
#2295=ORIENTED_EDGE('',*,*,#1736,.F.);
#2296=ORIENTED_EDGE('',*,*,#1737,.F.);
#2297=ORIENTED_EDGE('',*,*,#1738,.F.);
#2298=ORIENTED_EDGE('',*,*,#1739,.T.);
#2299=ORIENTED_EDGE('',*,*,#1740,.T.);
#2300=ORIENTED_EDGE('',*,*,#1734,.T.);
#2301=ORIENTED_EDGE('',*,*,#1741,.F.);
#2302=ORIENTED_EDGE('',*,*,#1738,.T.);
#2303=ORIENTED_EDGE('',*,*,#1742,.T.);
#2304=ORIENTED_EDGE('',*,*,#1743,.T.);
#2305=ORIENTED_EDGE('',*,*,#1744,.F.);
#2306=ORIENTED_EDGE('',*,*,#1745,.F.);
#2307=ORIENTED_EDGE('',*,*,#1746,.F.);
#2308=ORIENTED_EDGE('',*,*,#1744,.T.);
#2309=ORIENTED_EDGE('',*,*,#1747,.T.);
#2310=ORIENTED_EDGE('',*,*,#1748,.T.);
#2311=ORIENTED_EDGE('',*,*,#1749,.F.);
#2312=ORIENTED_EDGE('',*,*,#1750,.F.);
#2313=ORIENTED_EDGE('',*,*,#1751,.F.);
#2314=ORIENTED_EDGE('',*,*,#1749,.T.);
#2315=ORIENTED_EDGE('',*,*,#1752,.T.);
#2316=ORIENTED_EDGE('',*,*,#1753,.T.);
#2317=ORIENTED_EDGE('',*,*,#1726,.F.);
#2318=ORIENTED_EDGE('',*,*,#1754,.F.);
#2319=ORIENTED_EDGE('',*,*,#1755,.F.);
#2320=ORIENTED_EDGE('',*,*,#1756,.F.);
#2321=ORIENTED_EDGE('',*,*,#1757,.F.);
#2322=ORIENTED_EDGE('',*,*,#1758,.F.);
#2323=ORIENTED_EDGE('',*,*,#1759,.F.);
#2324=ORIENTED_EDGE('',*,*,#1760,.T.);
#2325=ORIENTED_EDGE('',*,*,#1761,.F.);
#2326=ORIENTED_EDGE('',*,*,#1725,.F.);
#2327=ORIENTED_EDGE('',*,*,#1762,.F.);
#2328=ORIENTED_EDGE('',*,*,#1763,.F.);
#2329=ORIENTED_EDGE('',*,*,#1764,.F.);
#2330=ORIENTED_EDGE('',*,*,#1765,.F.);
#2331=ORIENTED_EDGE('',*,*,#1766,.F.);
#2332=ORIENTED_EDGE('',*,*,#1767,.F.);
#2333=ORIENTED_EDGE('',*,*,#1723,.T.);
#2334=ORIENTED_EDGE('',*,*,#1731,.T.);
#2335=ORIENTED_EDGE('',*,*,#1763,.T.);
#2336=ORIENTED_EDGE('',*,*,#1754,.T.);
#2337=ORIENTED_EDGE('',*,*,#1730,.T.);
#2338=ORIENTED_EDGE('',*,*,#1736,.T.);
#2339=ORIENTED_EDGE('',*,*,#1764,.T.);
#2340=ORIENTED_EDGE('',*,*,#1735,.T.);
#2341=ORIENTED_EDGE('',*,*,#1740,.F.);
#2342=ORIENTED_EDGE('',*,*,#1765,.T.);
#2343=ORIENTED_EDGE('',*,*,#1746,.T.);
#2344=ORIENTED_EDGE('',*,*,#1766,.T.);
#2345=ORIENTED_EDGE('',*,*,#1739,.F.);
#2346=ORIENTED_EDGE('',*,*,#1745,.T.);
#2347=ORIENTED_EDGE('',*,*,#1751,.T.);
#2348=ORIENTED_EDGE('',*,*,#1767,.T.);
#2349=ORIENTED_EDGE('',*,*,#1750,.T.);
#2350=ORIENTED_EDGE('',*,*,#1755,.T.);
#2351=ORIENTED_EDGE('',*,*,#1762,.T.);
#2352=ORIENTED_EDGE('',*,*,#1757,.T.);
#2353=ORIENTED_EDGE('',*,*,#1752,.F.);
#2354=ORIENTED_EDGE('',*,*,#1748,.F.);
#2355=ORIENTED_EDGE('',*,*,#1758,.T.);
#2356=ORIENTED_EDGE('',*,*,#1747,.F.);
#2357=ORIENTED_EDGE('',*,*,#1743,.F.);
#2358=ORIENTED_EDGE('',*,*,#1737,.T.);
#2359=ORIENTED_EDGE('',*,*,#1759,.T.);
#2360=ORIENTED_EDGE('',*,*,#1742,.F.);
#2361=ORIENTED_EDGE('',*,*,#1760,.F.);
#2362=ORIENTED_EDGE('',*,*,#1741,.T.);
#2363=ORIENTED_EDGE('',*,*,#1733,.F.);
#2364=ORIENTED_EDGE('',*,*,#1761,.T.);
#2365=ORIENTED_EDGE('',*,*,#1732,.F.);
#2366=ORIENTED_EDGE('',*,*,#1728,.F.);
#2367=ORIENTED_EDGE('',*,*,#1753,.F.);
#2368=ORIENTED_EDGE('',*,*,#1756,.T.);
#2369=ORIENTED_EDGE('',*,*,#1727,.F.);
#2370=ORIENTED_EDGE('',*,*,#1768,.F.);
#2371=ORIENTED_EDGE('',*,*,#1769,.T.);
#2372=ORIENTED_EDGE('',*,*,#1770,.T.);
#2373=ORIENTED_EDGE('',*,*,#1769,.F.);
#2374=ORIENTED_EDGE('',*,*,#1771,.T.);
#2375=ORIENTED_EDGE('',*,*,#1772,.T.);
#2376=ORIENTED_EDGE('',*,*,#1773,.T.);
#2377=ORIENTED_EDGE('',*,*,#1774,.F.);
#2378=ORIENTED_EDGE('',*,*,#1775,.F.);
#2379=ORIENTED_EDGE('',*,*,#1776,.F.);
#2380=ORIENTED_EDGE('',*,*,#1774,.T.);
#2381=ORIENTED_EDGE('',*,*,#1777,.T.);
#2382=ORIENTED_EDGE('',*,*,#1778,.T.);
#2383=ORIENTED_EDGE('',*,*,#1779,.F.);
#2384=ORIENTED_EDGE('',*,*,#1780,.F.);
#2385=ORIENTED_EDGE('',*,*,#1781,.F.);
#2386=ORIENTED_EDGE('',*,*,#1782,.F.);
#2387=ORIENTED_EDGE('',*,*,#1783,.F.);
#2388=ORIENTED_EDGE('',*,*,#1784,.T.);
#2389=ORIENTED_EDGE('',*,*,#1785,.T.);
#2390=ORIENTED_EDGE('',*,*,#1779,.T.);
#2391=ORIENTED_EDGE('',*,*,#1786,.F.);
#2392=ORIENTED_EDGE('',*,*,#1783,.T.);
#2393=ORIENTED_EDGE('',*,*,#1787,.T.);
#2394=ORIENTED_EDGE('',*,*,#1788,.T.);
#2395=ORIENTED_EDGE('',*,*,#1789,.F.);
#2396=ORIENTED_EDGE('',*,*,#1790,.F.);
#2397=ORIENTED_EDGE('',*,*,#1791,.F.);
#2398=ORIENTED_EDGE('',*,*,#1789,.T.);
#2399=ORIENTED_EDGE('',*,*,#1792,.T.);
#2400=ORIENTED_EDGE('',*,*,#1793,.T.);
#2401=ORIENTED_EDGE('',*,*,#1794,.F.);
#2402=ORIENTED_EDGE('',*,*,#1795,.F.);
#2403=ORIENTED_EDGE('',*,*,#1796,.F.);
#2404=ORIENTED_EDGE('',*,*,#1794,.T.);
#2405=ORIENTED_EDGE('',*,*,#1797,.T.);
#2406=ORIENTED_EDGE('',*,*,#1798,.T.);
#2407=ORIENTED_EDGE('',*,*,#1771,.F.);
#2408=ORIENTED_EDGE('',*,*,#1799,.F.);
#2409=ORIENTED_EDGE('',*,*,#1800,.F.);
#2410=ORIENTED_EDGE('',*,*,#1801,.F.);
#2411=ORIENTED_EDGE('',*,*,#1802,.F.);
#2412=ORIENTED_EDGE('',*,*,#1803,.F.);
#2413=ORIENTED_EDGE('',*,*,#1804,.F.);
#2414=ORIENTED_EDGE('',*,*,#1805,.T.);
#2415=ORIENTED_EDGE('',*,*,#1806,.F.);
#2416=ORIENTED_EDGE('',*,*,#1770,.F.);
#2417=ORIENTED_EDGE('',*,*,#1807,.F.);
#2418=ORIENTED_EDGE('',*,*,#1808,.F.);
#2419=ORIENTED_EDGE('',*,*,#1809,.F.);
#2420=ORIENTED_EDGE('',*,*,#1810,.F.);
#2421=ORIENTED_EDGE('',*,*,#1811,.F.);
#2422=ORIENTED_EDGE('',*,*,#1812,.F.);
#2423=ORIENTED_EDGE('',*,*,#1768,.T.);
#2424=ORIENTED_EDGE('',*,*,#1776,.T.);
#2425=ORIENTED_EDGE('',*,*,#1808,.T.);
#2426=ORIENTED_EDGE('',*,*,#1799,.T.);
#2427=ORIENTED_EDGE('',*,*,#1775,.T.);
#2428=ORIENTED_EDGE('',*,*,#1781,.T.);
#2429=ORIENTED_EDGE('',*,*,#1809,.T.);
#2430=ORIENTED_EDGE('',*,*,#1780,.T.);
#2431=ORIENTED_EDGE('',*,*,#1785,.F.);
#2432=ORIENTED_EDGE('',*,*,#1810,.T.);
#2433=ORIENTED_EDGE('',*,*,#1791,.T.);
#2434=ORIENTED_EDGE('',*,*,#1811,.T.);
#2435=ORIENTED_EDGE('',*,*,#1784,.F.);
#2436=ORIENTED_EDGE('',*,*,#1790,.T.);
#2437=ORIENTED_EDGE('',*,*,#1796,.T.);
#2438=ORIENTED_EDGE('',*,*,#1812,.T.);
#2439=ORIENTED_EDGE('',*,*,#1795,.T.);
#2440=ORIENTED_EDGE('',*,*,#1800,.T.);
#2441=ORIENTED_EDGE('',*,*,#1807,.T.);
#2442=ORIENTED_EDGE('',*,*,#1802,.T.);
#2443=ORIENTED_EDGE('',*,*,#1797,.F.);
#2444=ORIENTED_EDGE('',*,*,#1793,.F.);
#2445=ORIENTED_EDGE('',*,*,#1803,.T.);
#2446=ORIENTED_EDGE('',*,*,#1792,.F.);
#2447=ORIENTED_EDGE('',*,*,#1788,.F.);
#2448=ORIENTED_EDGE('',*,*,#1782,.T.);
#2449=ORIENTED_EDGE('',*,*,#1804,.T.);
#2450=ORIENTED_EDGE('',*,*,#1787,.F.);
#2451=ORIENTED_EDGE('',*,*,#1805,.F.);
#2452=ORIENTED_EDGE('',*,*,#1786,.T.);
#2453=ORIENTED_EDGE('',*,*,#1778,.F.);
#2454=ORIENTED_EDGE('',*,*,#1806,.T.);
#2455=ORIENTED_EDGE('',*,*,#1777,.F.);
#2456=ORIENTED_EDGE('',*,*,#1773,.F.);
#2457=ORIENTED_EDGE('',*,*,#1798,.F.);
#2458=ORIENTED_EDGE('',*,*,#1801,.T.);
#2459=ORIENTED_EDGE('',*,*,#1772,.F.);
#2460=ORIENTED_EDGE('',*,*,#1813,.F.);
#2461=ORIENTED_EDGE('',*,*,#1814,.T.);
#2462=ORIENTED_EDGE('',*,*,#1815,.T.);
#2463=ORIENTED_EDGE('',*,*,#1814,.F.);
#2464=ORIENTED_EDGE('',*,*,#1816,.F.);
#2465=ORIENTED_EDGE('',*,*,#1817,.T.);
#2466=ORIENTED_EDGE('',*,*,#1818,.T.);
#2467=ORIENTED_EDGE('',*,*,#1817,.F.);
#2468=ORIENTED_EDGE('',*,*,#1819,.F.);
#2469=ORIENTED_EDGE('',*,*,#1820,.T.);
#2470=ORIENTED_EDGE('',*,*,#1821,.T.);
#2471=ORIENTED_EDGE('',*,*,#1820,.F.);
#2472=ORIENTED_EDGE('',*,*,#1822,.F.);
#2473=ORIENTED_EDGE('',*,*,#1823,.T.);
#2474=ORIENTED_EDGE('',*,*,#1824,.T.);
#2475=ORIENTED_EDGE('',*,*,#1823,.F.);
#2476=ORIENTED_EDGE('',*,*,#1825,.T.);
#2477=ORIENTED_EDGE('',*,*,#1826,.T.);
#2478=ORIENTED_EDGE('',*,*,#1827,.T.);
#2479=ORIENTED_EDGE('',*,*,#1826,.F.);
#2480=ORIENTED_EDGE('',*,*,#1828,.T.);
#2481=ORIENTED_EDGE('',*,*,#1829,.T.);
#2482=ORIENTED_EDGE('',*,*,#1830,.T.);
#2483=ORIENTED_EDGE('',*,*,#1829,.F.);
#2484=ORIENTED_EDGE('',*,*,#1831,.F.);
#2485=ORIENTED_EDGE('',*,*,#1832,.T.);
#2486=ORIENTED_EDGE('',*,*,#1833,.F.);
#2487=ORIENTED_EDGE('',*,*,#1832,.F.);
#2488=ORIENTED_EDGE('',*,*,#1834,.F.);
#2489=ORIENTED_EDGE('',*,*,#1835,.T.);
#2490=ORIENTED_EDGE('',*,*,#1836,.F.);
#2491=ORIENTED_EDGE('',*,*,#1835,.F.);
#2492=ORIENTED_EDGE('',*,*,#1837,.T.);
#2493=ORIENTED_EDGE('',*,*,#1838,.T.);
#2494=ORIENTED_EDGE('',*,*,#1839,.F.);
#2495=ORIENTED_EDGE('',*,*,#1840,.F.);
#2496=ORIENTED_EDGE('',*,*,#1841,.F.);
#2497=ORIENTED_EDGE('',*,*,#1842,.F.);
#2498=ORIENTED_EDGE('',*,*,#1843,.T.);
#2499=ORIENTED_EDGE('',*,*,#1844,.T.);
#2500=ORIENTED_EDGE('',*,*,#1845,.F.);
#2501=ORIENTED_EDGE('',*,*,#1846,.T.);
#2502=ORIENTED_EDGE('',*,*,#1847,.T.);
#2503=ORIENTED_EDGE('',*,*,#1848,.F.);
#2504=ORIENTED_EDGE('',*,*,#1849,.T.);
#2505=ORIENTED_EDGE('',*,*,#1850,.T.);
#2506=ORIENTED_EDGE('',*,*,#1851,.F.);
#2507=ORIENTED_EDGE('',*,*,#1852,.F.);
#2508=ORIENTED_EDGE('',*,*,#1845,.T.);
#2509=ORIENTED_EDGE('',*,*,#1853,.F.);
#2510=ORIENTED_EDGE('',*,*,#1837,.F.);
#2511=ORIENTED_EDGE('',*,*,#1854,.T.);
#2512=ORIENTED_EDGE('',*,*,#1827,.F.);
#2513=ORIENTED_EDGE('',*,*,#1830,.F.);
#2514=ORIENTED_EDGE('',*,*,#1848,.T.);
#2515=ORIENTED_EDGE('',*,*,#1855,.F.);
#2516=ORIENTED_EDGE('',*,*,#1838,.F.);
#2517=ORIENTED_EDGE('',*,*,#1853,.T.);
#2518=ORIENTED_EDGE('',*,*,#1813,.T.);
#2519=ORIENTED_EDGE('',*,*,#1816,.T.);
#2520=ORIENTED_EDGE('',*,*,#1847,.F.);
#2521=ORIENTED_EDGE('',*,*,#1856,.F.);
#2522=ORIENTED_EDGE('',*,*,#1839,.T.);
#2523=ORIENTED_EDGE('',*,*,#1855,.T.);
#2524=ORIENTED_EDGE('',*,*,#1831,.T.);
#2525=ORIENTED_EDGE('',*,*,#1834,.T.);
#2526=ORIENTED_EDGE('',*,*,#1846,.F.);
#2527=ORIENTED_EDGE('',*,*,#1854,.F.);
#2528=ORIENTED_EDGE('',*,*,#1840,.T.);
#2529=ORIENTED_EDGE('',*,*,#1856,.T.);
#2530=ORIENTED_EDGE('',*,*,#1821,.F.);
#2531=ORIENTED_EDGE('',*,*,#1824,.F.);
#2532=ORIENTED_EDGE('',*,*,#1849,.F.);
#2533=ORIENTED_EDGE('',*,*,#1857,.F.);
#2534=ORIENTED_EDGE('',*,*,#1842,.T.);
#2535=ORIENTED_EDGE('',*,*,#1858,.T.);
#2536=ORIENTED_EDGE('',*,*,#1825,.F.);
#2537=ORIENTED_EDGE('',*,*,#1828,.F.);
#2538=ORIENTED_EDGE('',*,*,#1850,.F.);
#2539=ORIENTED_EDGE('',*,*,#1858,.F.);
#2540=ORIENTED_EDGE('',*,*,#1841,.T.);
#2541=ORIENTED_EDGE('',*,*,#1859,.T.);
#2542=ORIENTED_EDGE('',*,*,#1815,.F.);
#2543=ORIENTED_EDGE('',*,*,#1818,.F.);
#2544=ORIENTED_EDGE('',*,*,#1851,.T.);
#2545=ORIENTED_EDGE('',*,*,#1859,.F.);
#2546=ORIENTED_EDGE('',*,*,#1844,.F.);
#2547=ORIENTED_EDGE('',*,*,#1860,.T.);
#2548=ORIENTED_EDGE('',*,*,#1833,.T.);
#2549=ORIENTED_EDGE('',*,*,#1836,.T.);
#2550=ORIENTED_EDGE('',*,*,#1852,.T.);
#2551=ORIENTED_EDGE('',*,*,#1860,.F.);
#2552=ORIENTED_EDGE('',*,*,#1843,.F.);
#2553=ORIENTED_EDGE('',*,*,#1857,.T.);
#2554=ORIENTED_EDGE('',*,*,#1819,.T.);
#2555=ORIENTED_EDGE('',*,*,#1822,.T.);
#2556=ORIENTED_EDGE('',*,*,#1861,.F.);
#2557=ORIENTED_EDGE('',*,*,#1862,.F.);
#2558=ORIENTED_EDGE('',*,*,#1863,.T.);
#2559=ORIENTED_EDGE('',*,*,#1864,.F.);
#2560=ORIENTED_EDGE('',*,*,#1863,.F.);
#2561=ORIENTED_EDGE('',*,*,#1865,.F.);
#2562=ORIENTED_EDGE('',*,*,#1866,.F.);
#2563=ORIENTED_EDGE('',*,*,#1867,.T.);
#2564=ORIENTED_EDGE('',*,*,#1868,.F.);
#2565=ORIENTED_EDGE('',*,*,#1867,.F.);
#2566=ORIENTED_EDGE('',*,*,#1869,.F.);
#2567=ORIENTED_EDGE('',*,*,#1870,.T.);
#2568=ORIENTED_EDGE('',*,*,#1871,.F.);
#2569=ORIENTED_EDGE('',*,*,#1870,.F.);
#2570=ORIENTED_EDGE('',*,*,#1872,.F.);
#2571=ORIENTED_EDGE('',*,*,#1873,.T.);
#2572=ORIENTED_EDGE('',*,*,#1874,.F.);
#2573=ORIENTED_EDGE('',*,*,#1873,.F.);
#2574=ORIENTED_EDGE('',*,*,#1861,.T.);
#2575=ORIENTED_EDGE('',*,*,#1862,.T.);
#2576=ORIENTED_EDGE('',*,*,#1875,.T.);
#2577=ORIENTED_EDGE('',*,*,#1872,.T.);
#2578=ORIENTED_EDGE('',*,*,#1875,.F.);
#2579=ORIENTED_EDGE('',*,*,#1876,.F.);
#2580=ORIENTED_EDGE('',*,*,#1877,.T.);
#2581=ORIENTED_EDGE('',*,*,#1869,.T.);
#2582=ORIENTED_EDGE('',*,*,#1877,.F.);
#2583=ORIENTED_EDGE('',*,*,#1865,.T.);
#2584=ORIENTED_EDGE('',*,*,#1866,.T.);
#2585=ORIENTED_EDGE('',*,*,#1878,.T.);
#2586=ORIENTED_EDGE('',*,*,#1879,.T.);
#2587=ORIENTED_EDGE('',*,*,#1878,.F.);
#2588=ORIENTED_EDGE('',*,*,#1871,.T.);
#2589=ORIENTED_EDGE('',*,*,#1874,.T.);
#2590=ORIENTED_EDGE('',*,*,#1876,.T.);
#2591=ORIENTED_EDGE('',*,*,#1864,.T.);
#2592=ORIENTED_EDGE('',*,*,#1879,.F.);
#2593=ORIENTED_EDGE('',*,*,#1868,.T.);
#2594=ORIENTED_EDGE('',*,*,#1880,.T.);
#2595=ORIENTED_EDGE('',*,*,#1881,.T.);
#2596=ORIENTED_EDGE('',*,*,#1882,.T.);
#2597=ORIENTED_EDGE('',*,*,#1883,.T.);
#2598=ORIENTED_EDGE('',*,*,#1884,.T.);
#2599=ORIENTED_EDGE('',*,*,#1885,.T.);
#2600=ORIENTED_EDGE('',*,*,#1886,.T.);
#2601=ORIENTED_EDGE('',*,*,#1880,.F.);
#2602=ORIENTED_EDGE('',*,*,#1887,.F.);
#2603=ORIENTED_EDGE('',*,*,#1888,.F.);
#2604=ORIENTED_EDGE('',*,*,#1889,.T.);
#2605=ORIENTED_EDGE('',*,*,#1890,.F.);
#2606=ORIENTED_EDGE('',*,*,#1889,.F.);
#2607=ORIENTED_EDGE('',*,*,#1891,.T.);
#2608=ORIENTED_EDGE('',*,*,#1892,.T.);
#2609=ORIENTED_EDGE('',*,*,#1893,.F.);
#2610=ORIENTED_EDGE('',*,*,#1892,.F.);
#2611=ORIENTED_EDGE('',*,*,#1894,.T.);
#2612=ORIENTED_EDGE('',*,*,#1891,.F.);
#2613=ORIENTED_EDGE('',*,*,#1895,.T.);
#2614=ORIENTED_EDGE('',*,*,#1896,.T.);
#2615=ORIENTED_EDGE('',*,*,#1895,.F.);
#2616=ORIENTED_EDGE('',*,*,#1894,.F.);
#2617=ORIENTED_EDGE('',*,*,#1887,.T.);
#2618=ORIENTED_EDGE('',*,*,#1888,.T.);
#2619=ORIENTED_EDGE('',*,*,#1897,.T.);
#2620=ORIENTED_EDGE('',*,*,#1898,.T.);
#2621=ORIENTED_EDGE('',*,*,#1897,.F.);
#2622=ORIENTED_EDGE('',*,*,#1898,.F.);
#2623=ORIENTED_EDGE('',*,*,#1899,.T.);
#2624=ORIENTED_EDGE('',*,*,#1900,.T.);
#2625=ORIENTED_EDGE('',*,*,#1899,.F.);
#2626=ORIENTED_EDGE('',*,*,#1893,.T.);
#2627=ORIENTED_EDGE('',*,*,#1901,.T.);
#2628=ORIENTED_EDGE('',*,*,#1902,.F.);
#2629=ORIENTED_EDGE('',*,*,#1903,.T.);
#2630=ORIENTED_EDGE('',*,*,#1904,.T.);
#2631=ORIENTED_EDGE('',*,*,#1905,.F.);
#2632=ORIENTED_EDGE('',*,*,#1906,.F.);
#2633=ORIENTED_EDGE('',*,*,#1900,.F.);
#2634=ORIENTED_EDGE('',*,*,#1896,.F.);
#2635=ORIENTED_EDGE('',*,*,#1890,.T.);
#2636=ORIENTED_EDGE('',*,*,#1901,.F.);
#2637=ORIENTED_EDGE('',*,*,#1907,.F.);
#2638=ORIENTED_EDGE('',*,*,#1908,.T.);
#2639=ORIENTED_EDGE('',*,*,#1909,.T.);
#2640=ORIENTED_EDGE('',*,*,#1910,.T.);
#2641=ORIENTED_EDGE('',*,*,#1902,.T.);
#2642=ORIENTED_EDGE('',*,*,#1910,.F.);
#2643=ORIENTED_EDGE('',*,*,#1911,.F.);
#2644=ORIENTED_EDGE('',*,*,#1912,.F.);
#2645=ORIENTED_EDGE('',*,*,#1913,.T.);
#2646=ORIENTED_EDGE('',*,*,#1903,.F.);
#2647=ORIENTED_EDGE('',*,*,#1913,.F.);
#2648=ORIENTED_EDGE('',*,*,#1914,.T.);
#2649=ORIENTED_EDGE('',*,*,#1915,.T.);
#2650=ORIENTED_EDGE('',*,*,#1916,.T.);
#2651=ORIENTED_EDGE('',*,*,#1904,.F.);
#2652=ORIENTED_EDGE('',*,*,#1916,.F.);
#2653=ORIENTED_EDGE('',*,*,#1917,.T.);
#2654=ORIENTED_EDGE('',*,*,#1918,.T.);
#2655=ORIENTED_EDGE('',*,*,#1919,.T.);
#2656=ORIENTED_EDGE('',*,*,#1905,.T.);
#2657=ORIENTED_EDGE('',*,*,#1919,.F.);
#2658=ORIENTED_EDGE('',*,*,#1920,.F.);
#2659=ORIENTED_EDGE('',*,*,#1921,.F.);
#2660=ORIENTED_EDGE('',*,*,#1922,.T.);
#2661=ORIENTED_EDGE('',*,*,#1906,.T.);
#2662=ORIENTED_EDGE('',*,*,#1922,.F.);
#2663=ORIENTED_EDGE('',*,*,#1923,.F.);
#2664=ORIENTED_EDGE('',*,*,#1924,.F.);
#2665=ORIENTED_EDGE('',*,*,#1907,.T.);
#2666=ORIENTED_EDGE('',*,*,#1920,.T.);
#2667=ORIENTED_EDGE('',*,*,#1918,.F.);
#2668=ORIENTED_EDGE('',*,*,#1881,.F.);
#2669=ORIENTED_EDGE('',*,*,#1917,.F.);
#2670=ORIENTED_EDGE('',*,*,#1915,.F.);
#2671=ORIENTED_EDGE('',*,*,#1882,.F.);
#2672=ORIENTED_EDGE('',*,*,#1914,.F.);
#2673=ORIENTED_EDGE('',*,*,#1912,.T.);
#2674=ORIENTED_EDGE('',*,*,#1883,.F.);
#2675=ORIENTED_EDGE('',*,*,#1911,.T.);
#2676=ORIENTED_EDGE('',*,*,#1909,.F.);
#2677=ORIENTED_EDGE('',*,*,#1884,.F.);
#2678=ORIENTED_EDGE('',*,*,#1908,.F.);
#2679=ORIENTED_EDGE('',*,*,#1924,.T.);
#2680=ORIENTED_EDGE('',*,*,#1885,.F.);
#2681=ORIENTED_EDGE('',*,*,#1923,.T.);
#2682=ORIENTED_EDGE('',*,*,#1921,.T.);
#2683=ORIENTED_EDGE('',*,*,#1886,.F.);
#2684=ORIENTED_EDGE('',*,*,#1925,.F.);
#2685=ORIENTED_EDGE('',*,*,#1926,.T.);
#2686=ORIENTED_EDGE('',*,*,#1927,.T.);
#2687=ORIENTED_EDGE('',*,*,#1926,.F.);
#2688=ORIENTED_EDGE('',*,*,#1928,.F.);
#2689=ORIENTED_EDGE('',*,*,#1929,.T.);
#2690=ORIENTED_EDGE('',*,*,#1930,.T.);
#2691=ORIENTED_EDGE('',*,*,#1929,.F.);
#2692=ORIENTED_EDGE('',*,*,#1927,.F.);
#2693=ORIENTED_EDGE('',*,*,#1928,.T.);
#2694=ORIENTED_EDGE('',*,*,#1925,.T.);
#2695=ORIENTED_EDGE('',*,*,#1930,.F.);
#2696=ORIENTED_EDGE('',*,*,#1931,.T.);
#2697=ORIENTED_EDGE('',*,*,#1932,.T.);
#2698=ORIENTED_EDGE('',*,*,#1933,.T.);
#2699=ORIENTED_EDGE('',*,*,#1934,.T.);
#2700=ORIENTED_EDGE('',*,*,#1935,.T.);
#2701=ORIENTED_EDGE('',*,*,#1936,.T.);
#2702=ORIENTED_EDGE('',*,*,#1937,.T.);
#2703=ORIENTED_EDGE('',*,*,#1931,.F.);
#2704=ORIENTED_EDGE('',*,*,#1938,.F.);
#2705=ORIENTED_EDGE('',*,*,#1939,.F.);
#2706=ORIENTED_EDGE('',*,*,#1940,.T.);
#2707=ORIENTED_EDGE('',*,*,#1941,.F.);
#2708=ORIENTED_EDGE('',*,*,#1940,.F.);
#2709=ORIENTED_EDGE('',*,*,#1942,.F.);
#2710=ORIENTED_EDGE('',*,*,#1943,.T.);
#2711=ORIENTED_EDGE('',*,*,#1944,.T.);
#2712=ORIENTED_EDGE('',*,*,#1943,.F.);
#2713=ORIENTED_EDGE('',*,*,#1938,.T.);
#2714=ORIENTED_EDGE('',*,*,#1939,.T.);
#2715=ORIENTED_EDGE('',*,*,#1945,.T.);
#2716=ORIENTED_EDGE('',*,*,#1942,.T.);
#2717=ORIENTED_EDGE('',*,*,#1945,.F.);
#2718=ORIENTED_EDGE('',*,*,#1946,.F.);
#2719=ORIENTED_EDGE('',*,*,#1947,.F.);
#2720=ORIENTED_EDGE('',*,*,#1948,.T.);
#2721=ORIENTED_EDGE('',*,*,#1949,.T.);
#2722=ORIENTED_EDGE('',*,*,#1948,.F.);
#2723=ORIENTED_EDGE('',*,*,#1946,.T.);
#2724=ORIENTED_EDGE('',*,*,#1947,.T.);
#2725=ORIENTED_EDGE('',*,*,#1950,.T.);
#2726=ORIENTED_EDGE('',*,*,#1951,.F.);
#2727=ORIENTED_EDGE('',*,*,#1950,.F.);
#2728=ORIENTED_EDGE('',*,*,#1951,.T.);
#2729=ORIENTED_EDGE('',*,*,#1952,.T.);
#2730=ORIENTED_EDGE('',*,*,#1953,.F.);
#2731=ORIENTED_EDGE('',*,*,#1954,.T.);
#2732=ORIENTED_EDGE('',*,*,#1955,.T.);
#2733=ORIENTED_EDGE('',*,*,#1956,.F.);
#2734=ORIENTED_EDGE('',*,*,#1957,.F.);
#2735=ORIENTED_EDGE('',*,*,#1949,.F.);
#2736=ORIENTED_EDGE('',*,*,#1941,.T.);
#2737=ORIENTED_EDGE('',*,*,#1944,.F.);
#2738=ORIENTED_EDGE('',*,*,#1952,.F.);
#2739=ORIENTED_EDGE('',*,*,#1958,.F.);
#2740=ORIENTED_EDGE('',*,*,#1959,.T.);
#2741=ORIENTED_EDGE('',*,*,#1960,.T.);
#2742=ORIENTED_EDGE('',*,*,#1961,.T.);
#2743=ORIENTED_EDGE('',*,*,#1953,.T.);
#2744=ORIENTED_EDGE('',*,*,#1961,.F.);
#2745=ORIENTED_EDGE('',*,*,#1962,.F.);
#2746=ORIENTED_EDGE('',*,*,#1963,.F.);
#2747=ORIENTED_EDGE('',*,*,#1964,.T.);
#2748=ORIENTED_EDGE('',*,*,#1954,.F.);
#2749=ORIENTED_EDGE('',*,*,#1964,.F.);
#2750=ORIENTED_EDGE('',*,*,#1965,.T.);
#2751=ORIENTED_EDGE('',*,*,#1966,.T.);
#2752=ORIENTED_EDGE('',*,*,#1967,.T.);
#2753=ORIENTED_EDGE('',*,*,#1955,.F.);
#2754=ORIENTED_EDGE('',*,*,#1967,.F.);
#2755=ORIENTED_EDGE('',*,*,#1968,.T.);
#2756=ORIENTED_EDGE('',*,*,#1969,.T.);
#2757=ORIENTED_EDGE('',*,*,#1970,.T.);
#2758=ORIENTED_EDGE('',*,*,#1956,.T.);
#2759=ORIENTED_EDGE('',*,*,#1970,.F.);
#2760=ORIENTED_EDGE('',*,*,#1971,.F.);
#2761=ORIENTED_EDGE('',*,*,#1972,.F.);
#2762=ORIENTED_EDGE('',*,*,#1973,.T.);
#2763=ORIENTED_EDGE('',*,*,#1957,.T.);
#2764=ORIENTED_EDGE('',*,*,#1973,.F.);
#2765=ORIENTED_EDGE('',*,*,#1974,.F.);
#2766=ORIENTED_EDGE('',*,*,#1975,.F.);
#2767=ORIENTED_EDGE('',*,*,#1958,.T.);
#2768=ORIENTED_EDGE('',*,*,#1934,.F.);
#2769=ORIENTED_EDGE('',*,*,#1965,.F.);
#2770=ORIENTED_EDGE('',*,*,#1963,.T.);
#2771=ORIENTED_EDGE('',*,*,#1933,.F.);
#2772=ORIENTED_EDGE('',*,*,#1968,.F.);
#2773=ORIENTED_EDGE('',*,*,#1966,.F.);
#2774=ORIENTED_EDGE('',*,*,#1932,.F.);
#2775=ORIENTED_EDGE('',*,*,#1971,.T.);
#2776=ORIENTED_EDGE('',*,*,#1969,.F.);
#2777=ORIENTED_EDGE('',*,*,#1937,.F.);
#2778=ORIENTED_EDGE('',*,*,#1974,.T.);
#2779=ORIENTED_EDGE('',*,*,#1972,.T.);
#2780=ORIENTED_EDGE('',*,*,#1936,.F.);
#2781=ORIENTED_EDGE('',*,*,#1959,.F.);
#2782=ORIENTED_EDGE('',*,*,#1975,.T.);
#2783=ORIENTED_EDGE('',*,*,#1935,.F.);
#2784=ORIENTED_EDGE('',*,*,#1962,.T.);
#2785=ORIENTED_EDGE('',*,*,#1960,.F.);
#2786=PLANE('',#3195);
#2787=PLANE('',#3200);
#2788=PLANE('',#3206);
#2789=PLANE('',#3208);
#2790=PLANE('',#3210);
#2791=PLANE('',#3212);
#2792=PLANE('',#3232);
#2793=PLANE('',#3234);
#2794=PLANE('',#3236);
#2795=PLANE('',#3237);
#2796=PLANE('',#3239);
#2797=PLANE('',#3274);
#2798=PLANE('',#3275);
#2799=PLANE('',#3276);
#2800=PLANE('',#3277);
#2801=PLANE('',#3295);
#2802=PLANE('',#3296);
#2803=PLANE('',#3300);
#2804=PLANE('',#3304);
#2805=PLANE('',#3308);
#2806=PLANE('',#3312);
#2807=PLANE('',#3313);
#2808=PLANE('',#3314);
#2809=PLANE('',#3315);
#2810=PLANE('',#3319);
#2811=PLANE('',#3320);
#2812=PLANE('',#3321);
#2813=PLANE('',#3322);
#2814=PLANE('',#3323);
#2815=PLANE('',#3324);
#2816=PLANE('',#3329);
#2817=PLANE('',#3330);
#2818=PLANE('',#3331);
#2819=PLANE('',#3332);
#2820=PLANE('',#3333);
#2821=PLANE('',#3334);
#2822=PLANE('',#3335);
#2823=PLANE('',#3342);
#2824=PLANE('',#3365);
#2825=PLANE('',#3366);
#2826=PLANE('',#3367);
#2827=PLANE('',#3368);
#2828=PLANE('',#3369);
#2829=PLANE('',#3370);
#2830=PLANE('',#3371);
#2831=PLANE('',#3378);
#2832=PLANE('',#3422);
#2833=PLANE('',#3423);
#2834=PLANE('',#3424);
#2835=PLANE('',#3425);
#2836=PLANE('',#3426);
#2837=PLANE('',#3427);
#2838=PLANE('',#3428);
#2839=PLANE('',#3429);
#2840=PLANE('',#3430);
#2841=PLANE('',#3431);
#2842=PLANE('',#3452);
#2843=PLANE('',#3453);
#2844=PLANE('',#3454);
#2845=PLANE('',#3455);
#2846=PLANE('',#3479);
#2847=PLANE('',#3480);
#2848=PLANE('',#3481);
#2849=PLANE('',#3482);
#2850=PLANE('',#3483);
#2851=PLANE('',#3484);
#2852=PLANE('',#3485);
#2853=PLANE('',#3486);
#2854=PLANE('',#3487);
#2855=PLANE('',#3488);
#2856=PLANE('',#3489);
#2857=PLANE('',#3490);
#2858=PLANE('',#3491);
#2859=PLANE('',#3492);
#2860=PLANE('',#3493);
#2861=PLANE('',#3501);
#2862=PLANE('',#3502);
#2863=PLANE('',#3526);
#2864=PLANE('',#3527);
#2865=PLANE('',#3528);
#2866=PLANE('',#3529);
#2867=PLANE('',#3530);
#2868=PLANE('',#3531);
#2869=PLANE('',#3532);
#2870=PLANE('',#3533);
#2871=PLANE('',#3534);
#2872=PLANE('',#3535);
#2873=PLANE('',#3536);
#2874=PLANE('',#3537);
#2875=PLANE('',#3538);
#2876=PLANE('',#3539);
#2877=PLANE('',#3540);
#2878=ADVANCED_FACE('',(#337,#271),#2786,.T.);
#2879=ADVANCED_FACE('',(#338,#272),#2787,.F.);
#2880=ADVANCED_FACE('',(#339),#220,.T.);
#2881=ADVANCED_FACE('',(#340),#2788,.F.);
#2882=ADVANCED_FACE('',(#341),#221,.T.);
#2883=ADVANCED_FACE('',(#342),#2789,.F.);
#2884=ADVANCED_FACE('',(#343),#222,.F.);
#2885=ADVANCED_FACE('',(#344),#2790,.T.);
#2886=ADVANCED_FACE('',(#345),#223,.F.);
#2887=ADVANCED_FACE('',(#346),#2791,.T.);
#2888=ADVANCED_FACE('',(#347),#224,.F.);
#2889=ADVANCED_FACE('',(#348),#225,.F.);
#2890=ADVANCED_FACE('',(#349),#226,.F.);
#2891=ADVANCED_FACE('',(#350),#227,.F.);
#2892=ADVANCED_FACE('',(#351),#228,.F.);
#2893=ADVANCED_FACE('',(#352),#229,.F.);
#2894=ADVANCED_FACE('',(#353,#273,#274,#275,#276,#277,#278),#2792,.T.);
#2895=ADVANCED_FACE('',(#354,#279,#280,#281,#282,#283,#284),#2793,.F.);
#2896=ADVANCED_FACE('',(#355),#2794,.F.);
#2897=ADVANCED_FACE('',(#356),#2795,.F.);
#2898=ADVANCED_FACE('',(#357),#230,.T.);
#2899=ADVANCED_FACE('',(#358),#2796,.F.);
#2900=ADVANCED_FACE('',(#359),#172,.F.);
#2901=ADVANCED_FACE('',(#360),#173,.T.);
#2902=ADVANCED_FACE('',(#361),#231,.F.);
#2903=ADVANCED_FACE('',(#362),#232,.F.);
#2904=ADVANCED_FACE('',(#363),#233,.F.);
#2905=ADVANCED_FACE('',(#364),#234,.F.);
#2906=ADVANCED_FACE('',(#365),#235,.F.);
#2907=ADVANCED_FACE('',(#366),#236,.F.);
#2908=ADVANCED_FACE('',(#367),#237,.T.);
#2909=ADVANCED_FACE('',(#368),#238,.F.);
#2910=ADVANCED_FACE('',(#369,#285,#286),#239,.F.);
#2911=ADVANCED_FACE('',(#370),#240,.T.);
#2912=ADVANCED_FACE('',(#371,#287,#288),#241,.T.);
#2913=ADVANCED_FACE('',(#372,#289),#2797,.T.);
#2914=ADVANCED_FACE('',(#373),#2798,.T.);
#2915=ADVANCED_FACE('',(#374,#290,#291,#292,#293,#294),#2799,.T.);
#2916=ADVANCED_FACE('',(#375,#295,#296,#297,#298),#2800,.F.);
#2917=ADVANCED_FACE('',(#376),#242,.F.);
#2918=ADVANCED_FACE('',(#377),#243,.F.);
#2919=ADVANCED_FACE('',(#378),#244,.T.);
#2920=ADVANCED_FACE('',(#379),#165,.F.);
#2921=ADVANCED_FACE('',(#380),#245,.F.);
#2922=ADVANCED_FACE('',(#381),#246,.T.);
#2923=ADVANCED_FACE('',(#382),#2801,.F.);
#2924=ADVANCED_FACE('',(#383),#2802,.F.);
#2925=ADVANCED_FACE('',(#384),#247,.T.);
#2926=ADVANCED_FACE('',(#385),#2803,.T.);
#2927=ADVANCED_FACE('',(#386),#248,.T.);
#2928=ADVANCED_FACE('',(#387),#2804,.T.);
#2929=ADVANCED_FACE('',(#388),#249,.T.);
#2930=ADVANCED_FACE('',(#389),#2805,.T.);
#2931=ADVANCED_FACE('',(#390),#250,.T.);
#2932=ADVANCED_FACE('',(#391),#2806,.T.);
#2933=ADVANCED_FACE('',(#392,#299,#300),#2807,.T.);
#2934=ADVANCED_FACE('',(#393,#301),#2808,.F.);
#2935=ADVANCED_FACE('',(#394,#302),#2809,.F.);
#2936=ADVANCED_FACE('',(#395),#251,.T.);
#2937=ADVANCED_FACE('',(#396),#2810,.F.);
#2938=ADVANCED_FACE('',(#397),#2811,.F.);
#2939=ADVANCED_FACE('',(#398,#303),#2812,.T.);
#2940=ADVANCED_FACE('',(#399,#304),#2813,.F.);
#2941=ADVANCED_FACE('',(#400,#305),#2814,.T.);
#2942=ADVANCED_FACE('',(#401,#306),#2815,.F.);
#2943=ADVANCED_FACE('',(#402),#252,.F.);
#2944=ADVANCED_FACE('',(#403),#2816,.T.);
#2945=ADVANCED_FACE('',(#404),#2817,.T.);
#2946=ADVANCED_FACE('',(#405),#2818,.F.);
#2947=ADVANCED_FACE('',(#406),#2819,.T.);
#2948=ADVANCED_FACE('',(#407),#2820,.T.);
#2949=ADVANCED_FACE('',(#408),#2821,.T.);
#2950=ADVANCED_FACE('',(#409,#307),#2822,.F.);
#2951=ADVANCED_FACE('',(#410,#308),#2823,.T.);
#2952=ADVANCED_FACE('',(#411),#83,.T.);
#2953=ADVANCED_FACE('',(#412),#84,.T.);
#2954=ADVANCED_FACE('',(#413),#85,.T.);
#2955=ADVANCED_FACE('',(#414),#86,.T.);
#2956=ADVANCED_FACE('',(#415),#87,.T.);
#2957=ADVANCED_FACE('',(#416),#88,.T.);
#2958=ADVANCED_FACE('',(#417),#89,.T.);
#2959=ADVANCED_FACE('',(#418),#90,.T.);
#2960=ADVANCED_FACE('',(#419),#91,.T.);
#2961=ADVANCED_FACE('',(#420),#92,.T.);
#2962=ADVANCED_FACE('',(#421),#93,.T.);
#2963=ADVANCED_FACE('',(#422),#94,.T.);
#2964=ADVANCED_FACE('',(#423),#253,.F.);
#2965=ADVANCED_FACE('',(#424),#2824,.T.);
#2966=ADVANCED_FACE('',(#425),#2825,.T.);
#2967=ADVANCED_FACE('',(#426),#2826,.F.);
#2968=ADVANCED_FACE('',(#427),#2827,.T.);
#2969=ADVANCED_FACE('',(#428),#2828,.T.);
#2970=ADVANCED_FACE('',(#429),#2829,.T.);
#2971=ADVANCED_FACE('',(#430,#309),#2830,.F.);
#2972=ADVANCED_FACE('',(#431,#310),#2831,.T.);
#2973=ADVANCED_FACE('',(#432),#95,.T.);
#2974=ADVANCED_FACE('',(#433),#96,.T.);
#2975=ADVANCED_FACE('',(#434),#97,.T.);
#2976=ADVANCED_FACE('',(#435),#98,.T.);
#2977=ADVANCED_FACE('',(#436),#99,.T.);
#2978=ADVANCED_FACE('',(#437),#100,.T.);
#2979=ADVANCED_FACE('',(#438),#101,.T.);
#2980=ADVANCED_FACE('',(#439),#102,.T.);
#2981=ADVANCED_FACE('',(#440),#103,.T.);
#2982=ADVANCED_FACE('',(#441),#104,.T.);
#2983=ADVANCED_FACE('',(#442),#105,.T.);
#2984=ADVANCED_FACE('',(#443),#106,.T.);
#2985=ADVANCED_FACE('',(#444),#254,.F.);
#2986=ADVANCED_FACE('',(#445),#255,.F.);
#2987=ADVANCED_FACE('',(#446),#256,.F.);
#2988=ADVANCED_FACE('',(#447),#257,.F.);
#2989=ADVANCED_FACE('',(#448),#258,.F.);
#2990=ADVANCED_FACE('',(#449),#259,.F.);
#2991=ADVANCED_FACE('',(#450),#260,.F.);
#2992=ADVANCED_FACE('',(#451),#261,.F.);
#2993=ADVANCED_FACE('',(#452,#311),#2832,.T.);
#2994=ADVANCED_FACE('',(#453,#312),#2833,.F.);
#2995=ADVANCED_FACE('',(#454,#313,#314),#2834,.F.);
#2996=ADVANCED_FACE('',(#455,#315,#316),#2835,.F.);
#2997=ADVANCED_FACE('',(#456,#317,#318),#2836,.T.);
#2998=ADVANCED_FACE('',(#457,#319,#320),#2837,.T.);
#2999=ADVANCED_FACE('',(#458,#321,#322),#2838,.T.);
#3000=ADVANCED_FACE('',(#459,#323,#324),#2839,.T.);
#3001=ADVANCED_FACE('',(#460,#325,#326),#2840,.F.);
#3002=ADVANCED_FACE('',(#461,#327,#328),#2841,.F.);
#3003=ADVANCED_FACE('',(#462),#107,.T.);
#3004=ADVANCED_FACE('',(#463),#108,.T.);
#3005=ADVANCED_FACE('',(#464),#109,.T.);
#3006=ADVANCED_FACE('',(#465),#110,.T.);
#3007=ADVANCED_FACE('',(#466),#262,.T.);
#3008=ADVANCED_FACE('',(#467),#263,.T.);
#3009=ADVANCED_FACE('',(#468),#264,.T.);
#3010=ADVANCED_FACE('',(#469),#2842,.T.);
#3011=ADVANCED_FACE('',(#470,#329),#2843,.T.);
#3012=ADVANCED_FACE('',(#471,#330),#2844,.F.);
#3013=ADVANCED_FACE('',(#472),#2845,.F.);
#3014=ADVANCED_FACE('',(#473),#111,.F.);
#3015=ADVANCED_FACE('',(#474),#174,.F.);
#3016=ADVANCED_FACE('',(#475),#112,.T.);
#3017=ADVANCED_FACE('',(#476),#265,.T.);
#3018=ADVANCED_FACE('',(#477),#266,.T.);
#3019=ADVANCED_FACE('',(#478),#113,.T.);
#3020=ADVANCED_FACE('',(#479,#331),#2846,.T.);
#3021=ADVANCED_FACE('',(#480),#2847,.T.);
#3022=ADVANCED_FACE('',(#481,#332),#2848,.T.);
#3023=ADVANCED_FACE('',(#482),#2849,.T.);
#3024=ADVANCED_FACE('',(#483),#2850,.F.);
#3025=ADVANCED_FACE('',(#484),#2851,.T.);
#3026=ADVANCED_FACE('',(#485),#2852,.T.);
#3027=ADVANCED_FACE('',(#486),#2853,.F.);
#3028=ADVANCED_FACE('',(#487),#2854,.F.);
#3029=ADVANCED_FACE('',(#488),#2855,.F.);
#3030=ADVANCED_FACE('',(#489),#2856,.F.);
#3031=ADVANCED_FACE('',(#490),#2857,.F.);
#3032=ADVANCED_FACE('',(#491),#2858,.F.);
#3033=ADVANCED_FACE('',(#492),#2859,.F.);
#3034=ADVANCED_FACE('',(#493),#2860,.F.);
#3035=ADVANCED_FACE('',(#494),#267,.T.);
#3036=ADVANCED_FACE('',(#495),#268,.F.);
#3037=ADVANCED_FACE('',(#496,#333),#2861,.F.);
#3038=ADVANCED_FACE('',(#497,#334),#2862,.F.);
#3039=ADVANCED_FACE('',(#498),#114,.F.);
#3040=ADVANCED_FACE('',(#499),#175,.F.);
#3041=ADVANCED_FACE('',(#500),#115,.T.);
#3042=ADVANCED_FACE('',(#501),#269,.T.);
#3043=ADVANCED_FACE('',(#502),#270,.T.);
#3044=ADVANCED_FACE('',(#503),#116,.T.);
#3045=ADVANCED_FACE('',(#504,#335),#2863,.T.);
#3046=ADVANCED_FACE('',(#505,#336),#2864,.T.);
#3047=ADVANCED_FACE('',(#506),#2865,.T.);
#3048=ADVANCED_FACE('',(#507),#2866,.T.);
#3049=ADVANCED_FACE('',(#508),#2867,.F.);
#3050=ADVANCED_FACE('',(#509),#2868,.T.);
#3051=ADVANCED_FACE('',(#510),#2869,.T.);
#3052=ADVANCED_FACE('',(#511),#2870,.F.);
#3053=ADVANCED_FACE('',(#512),#2871,.F.);
#3054=ADVANCED_FACE('',(#513),#2872,.T.);
#3055=ADVANCED_FACE('',(#514),#2873,.T.);
#3056=ADVANCED_FACE('',(#515),#2874,.T.);
#3057=ADVANCED_FACE('',(#516),#2875,.T.);
#3058=ADVANCED_FACE('',(#517),#2876,.T.);
#3059=ADVANCED_FACE('',(#518),#2877,.T.);
#3060=CLOSED_SHELL('',(#2878,#2879,#2880,#2881,#2882,#2883,#2884,#2885,
#2886,#2887));
#3061=CLOSED_SHELL('',(#2888,#2889,#2890,#2891,#2892,#2893,#2894,#2895,
#2896,#2897,#2898,#2899));
#3062=CLOSED_SHELL('',(#2900,#2901,#2902,#2903,#2904,#2905,#2906,#2907,
#2908,#2909,#2910,#2911,#2912,#2913,#2914,#2915,#2916));
#3063=CLOSED_SHELL('',(#2917,#2918,#2919,#2920,#2921,#2922,#2923,#2924,
#2925,#2926,#2927,#2928,#2929,#2930,#2931,#2932,#2933,#2934,#2935,#2936,
#2937,#2938,#2939,#2940,#2941,#2942));
#3064=CLOSED_SHELL('',(#2943,#2944,#2945,#2946,#2947,#2948,#2949,#2950,
#2951,#2952,#2953,#2954,#2955,#2956,#2957,#2958,#2959,#2960,#2961,#2962,
#2963));
#3065=CLOSED_SHELL('',(#2964,#2965,#2966,#2967,#2968,#2969,#2970,#2971,
#2972,#2973,#2974,#2975,#2976,#2977,#2978,#2979,#2980,#2981,#2982,#2983,
#2984));
#3066=CLOSED_SHELL('',(#2985,#2986,#2987,#2988,#2989,#2990,#2991,#2992,
#2993,#2994,#2995,#2996,#2997,#2998,#2999,#3000,#3001,#3002));
#3067=CLOSED_SHELL('',(#3003,#3004,#3005,#3006,#3007,#3008,#3009,#3010,
#3011,#3012,#3013));
#3068=CLOSED_SHELL('',(#3014,#3015,#3016,#3017,#3018,#3019,#3020,#3021,
#3022,#3023,#3024,#3025,#3026,#3027,#3028,#3029,#3030,#3031,#3032,#3033,
#3034));
#3069=CLOSED_SHELL('',(#3035,#3036,#3037,#3038));
#3070=CLOSED_SHELL('',(#3039,#3040,#3041,#3042,#3043,#3044,#3045,#3046,
#3047,#3048,#3049,#3050,#3051,#3052,#3053,#3054,#3055,#3056,#3057,#3058,
#3059));
#3071=DERIVED_UNIT_ELEMENT(#3093,1.);
#3072=DERIVED_UNIT_ELEMENT(#5660,-3.);
#3073=DERIVED_UNIT_ELEMENT(#3093,1.);
#3074=DERIVED_UNIT_ELEMENT(#5660,-3.);
#3075=DERIVED_UNIT_ELEMENT(#3093,1.);
#3076=DERIVED_UNIT_ELEMENT(#5660,-3.);
#3077=DERIVED_UNIT_ELEMENT(#3093,1.);
#3078=DERIVED_UNIT_ELEMENT(#5660,-3.);
#3079=DERIVED_UNIT_ELEMENT(#3093,1.);
#3080=DERIVED_UNIT_ELEMENT(#5660,-3.);
#3081=DERIVED_UNIT_ELEMENT(#3093,1.);
#3082=DERIVED_UNIT_ELEMENT(#5660,-3.);
#3083=DERIVED_UNIT_ELEMENT(#3093,1.);
#3084=DERIVED_UNIT_ELEMENT(#5660,-3.);
#3085=DERIVED_UNIT_ELEMENT(#3093,1.);
#3086=DERIVED_UNIT_ELEMENT(#5660,-3.);
#3087=DERIVED_UNIT_ELEMENT(#3093,1.);
#3088=DERIVED_UNIT_ELEMENT(#5660,-3.);
#3089=DERIVED_UNIT_ELEMENT(#3093,1.);
#3090=DERIVED_UNIT_ELEMENT(#5660,-3.);
#3091=DERIVED_UNIT_ELEMENT(#3093,1.);
#3092=DERIVED_UNIT_ELEMENT(#5660,-3.);
#3093=(
MASS_UNIT()
NAMED_UNIT(*)
SI_UNIT(.KILO.,.GRAM.)
);
#3094=DERIVED_UNIT((#3071,#3072));
#3095=DERIVED_UNIT((#3073,#3074));
#3096=DERIVED_UNIT((#3075,#3076));
#3097=DERIVED_UNIT((#3077,#3078));
#3098=DERIVED_UNIT((#3079,#3080));
#3099=DERIVED_UNIT((#3081,#3082));
#3100=DERIVED_UNIT((#3083,#3084));
#3101=DERIVED_UNIT((#3085,#3086));
#3102=DERIVED_UNIT((#3087,#3088));
#3103=DERIVED_UNIT((#3089,#3090));
#3104=DERIVED_UNIT((#3091,#3092));
#3105=MEASURE_REPRESENTATION_ITEM('density measure',
POSITIVE_RATIO_MEASURE(7850.),#3094);
#3106=MEASURE_REPRESENTATION_ITEM('density measure',
POSITIVE_RATIO_MEASURE(7850.),#3095);
#3107=MEASURE_REPRESENTATION_ITEM('density measure',
POSITIVE_RATIO_MEASURE(7850.),#3096);
#3108=MEASURE_REPRESENTATION_ITEM('density measure',
POSITIVE_RATIO_MEASURE(7850.),#3097);
#3109=MEASURE_REPRESENTATION_ITEM('density measure',
POSITIVE_RATIO_MEASURE(7850.),#3098);
#3110=MEASURE_REPRESENTATION_ITEM('density measure',
POSITIVE_RATIO_MEASURE(7850.),#3099);
#3111=MEASURE_REPRESENTATION_ITEM('density measure',
POSITIVE_RATIO_MEASURE(7850.),#3100);
#3112=MEASURE_REPRESENTATION_ITEM('density measure',
POSITIVE_RATIO_MEASURE(7850.),#3101);
#3113=MEASURE_REPRESENTATION_ITEM('density measure',
POSITIVE_RATIO_MEASURE(7850.),#3102);
#3114=MEASURE_REPRESENTATION_ITEM('density measure',
POSITIVE_RATIO_MEASURE(7850.),#3103);
#3115=MEASURE_REPRESENTATION_ITEM('density measure',
POSITIVE_RATIO_MEASURE(7850.),#3104);
#3116=PROPERTY_DEFINITION_REPRESENTATION(#3171,#3138);
#3117=PROPERTY_DEFINITION_REPRESENTATION(#3172,#3139);
#3118=PROPERTY_DEFINITION_REPRESENTATION(#3173,#3140);
#3119=PROPERTY_DEFINITION_REPRESENTATION(#3174,#3141);
#3120=PROPERTY_DEFINITION_REPRESENTATION(#3175,#3142);
#3121=PROPERTY_DEFINITION_REPRESENTATION(#3176,#3143);
#3122=PROPERTY_DEFINITION_REPRESENTATION(#3177,#3144);
#3123=PROPERTY_DEFINITION_REPRESENTATION(#3178,#3145);
#3124=PROPERTY_DEFINITION_REPRESENTATION(#3179,#3146);
#3125=PROPERTY_DEFINITION_REPRESENTATION(#3180,#3147);
#3126=PROPERTY_DEFINITION_REPRESENTATION(#3181,#3148);
#3127=PROPERTY_DEFINITION_REPRESENTATION(#3182,#3149);
#3128=PROPERTY_DEFINITION_REPRESENTATION(#3183,#3150);
#3129=PROPERTY_DEFINITION_REPRESENTATION(#3184,#3151);
#3130=PROPERTY_DEFINITION_REPRESENTATION(#3185,#3152);
#3131=PROPERTY_DEFINITION_REPRESENTATION(#3186,#3153);
#3132=PROPERTY_DEFINITION_REPRESENTATION(#3187,#3154);
#3133=PROPERTY_DEFINITION_REPRESENTATION(#3188,#3155);
#3134=PROPERTY_DEFINITION_REPRESENTATION(#3189,#3156);
#3135=PROPERTY_DEFINITION_REPRESENTATION(#3190,#3157);
#3136=PROPERTY_DEFINITION_REPRESENTATION(#3191,#3158);
#3137=PROPERTY_DEFINITION_REPRESENTATION(#3192,#3159);
#3138=REPRESENTATION('material name',(#3160),#5647);
#3139=REPRESENTATION('density',(#3105),#5647);
#3140=REPRESENTATION('material name',(#3161),#5648);
#3141=REPRESENTATION('density',(#3106),#5648);
#3142=REPRESENTATION('material name',(#3162),#5649);
#3143=REPRESENTATION('density',(#3107),#5649);
#3144=REPRESENTATION('material name',(#3163),#5650);
#3145=REPRESENTATION('density',(#3108),#5650);
#3146=REPRESENTATION('material name',(#3164),#5651);
#3147=REPRESENTATION('density',(#3109),#5651);
#3148=REPRESENTATION('material name',(#3165),#5652);
#3149=REPRESENTATION('density',(#3110),#5652);
#3150=REPRESENTATION('material name',(#3166),#5653);
#3151=REPRESENTATION('density',(#3111),#5653);
#3152=REPRESENTATION('material name',(#3167),#5654);
#3153=REPRESENTATION('density',(#3112),#5654);
#3154=REPRESENTATION('material name',(#3168),#5655);
#3155=REPRESENTATION('density',(#3113),#5655);
#3156=REPRESENTATION('material name',(#3169),#5656);
#3157=REPRESENTATION('density',(#3114),#5656);
#3158=REPRESENTATION('material name',(#3170),#5657);
#3159=REPRESENTATION('density',(#3115),#5657);
#3160=DESCRIPTIVE_REPRESENTATION_ITEM('Steel','Steel');
#3161=DESCRIPTIVE_REPRESENTATION_ITEM('Steel','Steel');
#3162=DESCRIPTIVE_REPRESENTATION_ITEM('Steel','Steel');
#3163=DESCRIPTIVE_REPRESENTATION_ITEM('Steel','Steel');
#3164=DESCRIPTIVE_REPRESENTATION_ITEM('Steel','Steel');
#3165=DESCRIPTIVE_REPRESENTATION_ITEM('Steel','Steel');
#3166=DESCRIPTIVE_REPRESENTATION_ITEM('Steel','Steel');
#3167=DESCRIPTIVE_REPRESENTATION_ITEM('Steel','Steel');
#3168=DESCRIPTIVE_REPRESENTATION_ITEM('Steel','Steel');
#3169=DESCRIPTIVE_REPRESENTATION_ITEM('Steel','Steel');
#3170=DESCRIPTIVE_REPRESENTATION_ITEM('Steel','Steel');
#3171=PROPERTY_DEFINITION('material property','material name',#5719);
#3172=PROPERTY_DEFINITION('material property','density of part',#5719);
#3173=PROPERTY_DEFINITION('material property','material name',#5720);
#3174=PROPERTY_DEFINITION('material property','density of part',#5720);
#3175=PROPERTY_DEFINITION('material property','material name',#5721);
#3176=PROPERTY_DEFINITION('material property','density of part',#5721);
#3177=PROPERTY_DEFINITION('material property','material name',#5722);
#3178=PROPERTY_DEFINITION('material property','density of part',#5722);
#3179=PROPERTY_DEFINITION('material property','material name',#5723);
#3180=PROPERTY_DEFINITION('material property','density of part',#5723);
#3181=PROPERTY_DEFINITION('material property','material name',#5724);
#3182=PROPERTY_DEFINITION('material property','density of part',#5724);
#3183=PROPERTY_DEFINITION('material property','material name',#5725);
#3184=PROPERTY_DEFINITION('material property','density of part',#5725);
#3185=PROPERTY_DEFINITION('material property','material name',#5726);
#3186=PROPERTY_DEFINITION('material property','density of part',#5726);
#3187=PROPERTY_DEFINITION('material property','material name',#5727);
#3188=PROPERTY_DEFINITION('material property','density of part',#5727);
#3189=PROPERTY_DEFINITION('material property','material name',#5728);
#3190=PROPERTY_DEFINITION('material property','density of part',#5728);
#3191=PROPERTY_DEFINITION('material property','material name',#5729);
#3192=PROPERTY_DEFINITION('material property','density of part',#5729);
#3193=AXIS2_PLACEMENT_3D('',#4487,#3559,#3560);
#3194=AXIS2_PLACEMENT_3D('',#4488,#3561,#3562);
#3195=AXIS2_PLACEMENT_3D('',#4489,#3563,#3564);
#3196=AXIS2_PLACEMENT_3D('',#4492,#3565,#3566);
#3197=AXIS2_PLACEMENT_3D('',#4496,#3568,#3569);
#3198=AXIS2_PLACEMENT_3D('',#4502,#3572,#3573);
#3199=AXIS2_PLACEMENT_3D('',#4505,#3575,#3576);
#3200=AXIS2_PLACEMENT_3D('',#4506,#3577,#3578);
#3201=AXIS2_PLACEMENT_3D('',#4509,#3579,#3580);
#3202=AXIS2_PLACEMENT_3D('',#4513,#3582,#3583);
#3203=AXIS2_PLACEMENT_3D('',#4517,#3585,#3586);
#3204=AXIS2_PLACEMENT_3D('',#4521,#3588,#3589);
#3205=AXIS2_PLACEMENT_3D('',#4523,#3591,#3592);
#3206=AXIS2_PLACEMENT_3D('',#4526,#3595,#3596);
#3207=AXIS2_PLACEMENT_3D('',#4528,#3598,#3599);
#3208=AXIS2_PLACEMENT_3D('',#4530,#3601,#3602);
#3209=AXIS2_PLACEMENT_3D('',#4531,#3603,#3604);
#3210=AXIS2_PLACEMENT_3D('',#4534,#3607,#3608);
#3211=AXIS2_PLACEMENT_3D('',#4536,#3610,#3611);
#3212=AXIS2_PLACEMENT_3D('',#4538,#3613,#3614);
#3213=AXIS2_PLACEMENT_3D('',#4539,#3615,#3616);
#3214=AXIS2_PLACEMENT_3D('',#4540,#3617,#3618);
#3215=AXIS2_PLACEMENT_3D('',#4542,#3619,#3620);
#3216=AXIS2_PLACEMENT_3D('',#4545,#3622,#3623);
#3217=AXIS2_PLACEMENT_3D('',#4546,#3624,#3625);
#3218=AXIS2_PLACEMENT_3D('',#4548,#3626,#3627);
#3219=AXIS2_PLACEMENT_3D('',#4551,#3629,#3630);
#3220=AXIS2_PLACEMENT_3D('',#4552,#3631,#3632);
#3221=AXIS2_PLACEMENT_3D('',#4554,#3633,#3634);
#3222=AXIS2_PLACEMENT_3D('',#4557,#3636,#3637);
#3223=AXIS2_PLACEMENT_3D('',#4558,#3638,#3639);
#3224=AXIS2_PLACEMENT_3D('',#4560,#3640,#3641);
#3225=AXIS2_PLACEMENT_3D('',#4563,#3643,#3644);
#3226=AXIS2_PLACEMENT_3D('',#4564,#3645,#3646);
#3227=AXIS2_PLACEMENT_3D('',#4566,#3647,#3648);
#3228=AXIS2_PLACEMENT_3D('',#4569,#3650,#3651);
#3229=AXIS2_PLACEMENT_3D('',#4570,#3652,#3653);
#3230=AXIS2_PLACEMENT_3D('',#4572,#3654,#3655);
#3231=AXIS2_PLACEMENT_3D('',#4575,#3657,#3658);
#3232=AXIS2_PLACEMENT_3D('',#4576,#3659,#3660);
#3233=AXIS2_PLACEMENT_3D('',#4583,#3663,#3664);
#3234=AXIS2_PLACEMENT_3D('',#4585,#3666,#3667);
#3235=AXIS2_PLACEMENT_3D('',#4592,#3670,#3671);
#3236=AXIS2_PLACEMENT_3D('',#4594,#3673,#3674);
#3237=AXIS2_PLACEMENT_3D('',#4597,#3677,#3678);
#3238=AXIS2_PLACEMENT_3D('',#4599,#3680,#3681);
#3239=AXIS2_PLACEMENT_3D('',#4601,#3683,#3684);
#3240=AXIS2_PLACEMENT_3D('',#4602,#3685,#3686);
#3241=AXIS2_PLACEMENT_3D('',#4603,#3687,#3688);
#3242=AXIS2_PLACEMENT_3D('',#4605,#3689,#3690);
#3243=AXIS2_PLACEMENT_3D('',#4607,#3691,#3692);
#3244=AXIS2_PLACEMENT_3D('',#4608,#3693,#3694);
#3245=AXIS2_PLACEMENT_3D('',#4609,#3695,#3696);
#3246=AXIS2_PLACEMENT_3D('',#4611,#3697,#3698);
#3247=AXIS2_PLACEMENT_3D('',#4613,#3699,#3700);
#3248=AXIS2_PLACEMENT_3D('',#4614,#3701,#3702);
#3249=AXIS2_PLACEMENT_3D('',#4615,#3703,#3704);
#3250=AXIS2_PLACEMENT_3D('',#4698,#3706,#3707);
#3251=AXIS2_PLACEMENT_3D('',#4781,#3709,#3710);
#3252=AXIS2_PLACEMENT_3D('',#4783,#3711,#3712);
#3253=AXIS2_PLACEMENT_3D('',#4786,#3714,#3715);
#3254=AXIS2_PLACEMENT_3D('',#4787,#3716,#3717);
#3255=AXIS2_PLACEMENT_3D('',#4789,#3718,#3719);
#3256=AXIS2_PLACEMENT_3D('',#4792,#3721,#3722);
#3257=AXIS2_PLACEMENT_3D('',#4793,#3723,#3724);
#3258=AXIS2_PLACEMENT_3D('',#4795,#3725,#3726);
#3259=AXIS2_PLACEMENT_3D('',#4798,#3728,#3729);
#3260=AXIS2_PLACEMENT_3D('',#4799,#3730,#3731);
#3261=AXIS2_PLACEMENT_3D('',#4801,#3732,#3733);
#3262=AXIS2_PLACEMENT_3D('',#4804,#3735,#3736);
#3263=AXIS2_PLACEMENT_3D('',#4805,#3737,#3738);
#3264=AXIS2_PLACEMENT_3D('',#4807,#3739,#3740);
#3265=AXIS2_PLACEMENT_3D('',#4810,#3742,#3743);
#3266=AXIS2_PLACEMENT_3D('',#4811,#3744,#3745);
#3267=AXIS2_PLACEMENT_3D('',#4814,#3747,#3748);
#3268=AXIS2_PLACEMENT_3D('',#4815,#3749,#3750);
#3269=AXIS2_PLACEMENT_3D('',#4817,#3751,#3752);
#3270=AXIS2_PLACEMENT_3D('',#4819,#3754,#3755);
#3271=AXIS2_PLACEMENT_3D('',#4821,#3756,#3757);
#3272=AXIS2_PLACEMENT_3D('',#4823,#3759,#3760);
#3273=AXIS2_PLACEMENT_3D('',#4826,#3762,#3763);
#3274=AXIS2_PLACEMENT_3D('',#4827,#3764,#3765);
#3275=AXIS2_PLACEMENT_3D('',#4828,#3766,#3767);
#3276=AXIS2_PLACEMENT_3D('',#4829,#3768,#3769);
#3277=AXIS2_PLACEMENT_3D('',#4830,#3770,#3771);
#3278=AXIS2_PLACEMENT_3D('',#4831,#3772,#3773);
#3279=AXIS2_PLACEMENT_3D('',#4832,#3774,#3775);
#3280=AXIS2_PLACEMENT_3D('',#4834,#3776,#3777);
#3281=AXIS2_PLACEMENT_3D('',#4837,#3779,#3780);
#3282=AXIS2_PLACEMENT_3D('',#4838,#3781,#3782);
#3283=AXIS2_PLACEMENT_3D('',#4840,#3783,#3784);
#3284=AXIS2_PLACEMENT_3D('',#4843,#3786,#3787);
#3285=AXIS2_PLACEMENT_3D('',#4844,#3788,#3789);
#3286=AXIS2_PLACEMENT_3D('',#4846,#3790,#3791);
#3287=AXIS2_PLACEMENT_3D('',#4849,#3793,#3794);
#3288=AXIS2_PLACEMENT_3D('',#4878,#3795,#3796);
#3289=AXIS2_PLACEMENT_3D('',#4880,#3797,#3798);
#3290=AXIS2_PLACEMENT_3D('',#4881,#3799,#3800);
#3291=AXIS2_PLACEMENT_3D('',#4883,#3801,#3802);
#3292=AXIS2_PLACEMENT_3D('',#4885,#3804,#3805);
#3293=AXIS2_PLACEMENT_3D('',#4888,#3806,#3807);
#3294=AXIS2_PLACEMENT_3D('',#4892,#3809,#3810);
#3295=AXIS2_PLACEMENT_3D('',#4894,#3812,#3813);
#3296=AXIS2_PLACEMENT_3D('',#4900,#3817,#3818);
#3297=AXIS2_PLACEMENT_3D('',#4906,#3822,#3823);
#3298=AXIS2_PLACEMENT_3D('',#4909,#3824,#3825);
#3299=AXIS2_PLACEMENT_3D('',#4913,#3827,#3828);
#3300=AXIS2_PLACEMENT_3D('',#4915,#3830,#3831);
#3301=AXIS2_PLACEMENT_3D('',#4921,#3835,#3836);
#3302=AXIS2_PLACEMENT_3D('',#4923,#3837,#3838);
#3303=AXIS2_PLACEMENT_3D('',#4926,#3840,#3841);
#3304=AXIS2_PLACEMENT_3D('',#4927,#3842,#3843);
#3305=AXIS2_PLACEMENT_3D('',#4933,#3847,#3848);
#3306=AXIS2_PLACEMENT_3D('',#4935,#3849,#3850);
#3307=AXIS2_PLACEMENT_3D('',#4938,#3852,#3853);
#3308=AXIS2_PLACEMENT_3D('',#4939,#3854,#3855);
#3309=AXIS2_PLACEMENT_3D('',#4945,#3859,#3860);
#3310=AXIS2_PLACEMENT_3D('',#4947,#3861,#3862);
#3311=AXIS2_PLACEMENT_3D('',#4950,#3864,#3865);
#3312=AXIS2_PLACEMENT_3D('',#4951,#3866,#3867);
#3313=AXIS2_PLACEMENT_3D('',#4954,#3870,#3871);
#3314=AXIS2_PLACEMENT_3D('',#4965,#3878,#3879);
#3315=AXIS2_PLACEMENT_3D('',#4966,#3880,#3881);
#3316=AXIS2_PLACEMENT_3D('',#4967,#3882,#3883);
#3317=AXIS2_PLACEMENT_3D('',#4972,#3885,#3886);
#3318=AXIS2_PLACEMENT_3D('',#4975,#3888,#3889);
#3319=AXIS2_PLACEMENT_3D('',#4976,#3890,#3891);
#3320=AXIS2_PLACEMENT_3D('',#4979,#3894,#3895);
#3321=AXIS2_PLACEMENT_3D('',#4982,#3898,#3899);
#3322=AXIS2_PLACEMENT_3D('',#4983,#3900,#3901);
#3323=AXIS2_PLACEMENT_3D('',#4984,#3902,#3903);
#3324=AXIS2_PLACEMENT_3D('',#4985,#3904,#3905);
#3325=AXIS2_PLACEMENT_3D('',#4986,#3906,#3907);
#3326=AXIS2_PLACEMENT_3D('',#4987,#3908,#3909);
#3327=AXIS2_PLACEMENT_3D('',#4989,#3910,#3911);
#3328=AXIS2_PLACEMENT_3D('',#4992,#3913,#3914);
#3329=AXIS2_PLACEMENT_3D('',#4993,#3915,#3916);
#3330=AXIS2_PLACEMENT_3D('',#5014,#3919,#3920);
#3331=AXIS2_PLACEMENT_3D('',#5032,#3922,#3923);
#3332=AXIS2_PLACEMENT_3D('',#5050,#3925,#3926);
#3333=AXIS2_PLACEMENT_3D('',#5068,#3928,#3929);
#3334=AXIS2_PLACEMENT_3D('',#5086,#3931,#3932);
#3335=AXIS2_PLACEMENT_3D('',#5101,#3933,#3934);
#3336=AXIS2_PLACEMENT_3D('',#5102,#3935,#3936);
#3337=AXIS2_PLACEMENT_3D('',#5103,#3937,#3938);
#3338=AXIS2_PLACEMENT_3D('',#5104,#3939,#3940);
#3339=AXIS2_PLACEMENT_3D('',#5105,#3941,#3942);
#3340=AXIS2_PLACEMENT_3D('',#5106,#3943,#3944);
#3341=AXIS2_PLACEMENT_3D('',#5107,#3945,#3946);
#3342=AXIS2_PLACEMENT_3D('',#5108,#3947,#3948);
#3343=AXIS2_PLACEMENT_3D('',#5109,#3949,#3950);
#3344=AXIS2_PLACEMENT_3D('',#5110,#3951,#3952);
#3345=AXIS2_PLACEMENT_3D('',#5111,#3953,#3954);
#3346=AXIS2_PLACEMENT_3D('',#5112,#3955,#3956);
#3347=AXIS2_PLACEMENT_3D('',#5113,#3957,#3958);
#3348=AXIS2_PLACEMENT_3D('',#5114,#3959,#3960);
#3349=AXIS2_PLACEMENT_3D('',#5115,#3961,#3962);
#3350=AXIS2_PLACEMENT_3D('',#5116,#3963,#3964);
#3351=AXIS2_PLACEMENT_3D('',#5117,#3965,#3966);
#3352=AXIS2_PLACEMENT_3D('',#5118,#3967,#3968);
#3353=AXIS2_PLACEMENT_3D('',#5119,#3969,#3970);
#3354=AXIS2_PLACEMENT_3D('',#5120,#3971,#3972);
#3355=AXIS2_PLACEMENT_3D('',#5121,#3973,#3974);
#3356=AXIS2_PLACEMENT_3D('',#5122,#3975,#3976);
#3357=AXIS2_PLACEMENT_3D('',#5123,#3977,#3978);
#3358=AXIS2_PLACEMENT_3D('',#5124,#3979,#3980);
#3359=AXIS2_PLACEMENT_3D('',#5125,#3981,#3982);
#3360=AXIS2_PLACEMENT_3D('',#5126,#3983,#3984);
#3361=AXIS2_PLACEMENT_3D('',#5127,#3985,#3986);
#3362=AXIS2_PLACEMENT_3D('',#5128,#3987,#3988);
#3363=AXIS2_PLACEMENT_3D('',#5130,#3989,#3990);
#3364=AXIS2_PLACEMENT_3D('',#5133,#3992,#3993);
#3365=AXIS2_PLACEMENT_3D('',#5134,#3994,#3995);
#3366=AXIS2_PLACEMENT_3D('',#5155,#3998,#3999);
#3367=AXIS2_PLACEMENT_3D('',#5173,#4001,#4002);
#3368=AXIS2_PLACEMENT_3D('',#5191,#4004,#4005);
#3369=AXIS2_PLACEMENT_3D('',#5209,#4007,#4008);
#3370=AXIS2_PLACEMENT_3D('',#5227,#4010,#4011);
#3371=AXIS2_PLACEMENT_3D('',#5242,#4012,#4013);
#3372=AXIS2_PLACEMENT_3D('',#5243,#4014,#4015);
#3373=AXIS2_PLACEMENT_3D('',#5244,#4016,#4017);
#3374=AXIS2_PLACEMENT_3D('',#5245,#4018,#4019);
#3375=AXIS2_PLACEMENT_3D('',#5246,#4020,#4021);
#3376=AXIS2_PLACEMENT_3D('',#5247,#4022,#4023);
#3377=AXIS2_PLACEMENT_3D('',#5248,#4024,#4025);
#3378=AXIS2_PLACEMENT_3D('',#5249,#4026,#4027);
#3379=AXIS2_PLACEMENT_3D('',#5250,#4028,#4029);
#3380=AXIS2_PLACEMENT_3D('',#5251,#4030,#4031);
#3381=AXIS2_PLACEMENT_3D('',#5252,#4032,#4033);
#3382=AXIS2_PLACEMENT_3D('',#5253,#4034,#4035);
#3383=AXIS2_PLACEMENT_3D('',#5254,#4036,#4037);
#3384=AXIS2_PLACEMENT_3D('',#5255,#4038,#4039);
#3385=AXIS2_PLACEMENT_3D('',#5256,#4040,#4041);
#3386=AXIS2_PLACEMENT_3D('',#5257,#4042,#4043);
#3387=AXIS2_PLACEMENT_3D('',#5258,#4044,#4045);
#3388=AXIS2_PLACEMENT_3D('',#5259,#4046,#4047);
#3389=AXIS2_PLACEMENT_3D('',#5260,#4048,#4049);
#3390=AXIS2_PLACEMENT_3D('',#5261,#4050,#4051);
#3391=AXIS2_PLACEMENT_3D('',#5262,#4052,#4053);
#3392=AXIS2_PLACEMENT_3D('',#5263,#4054,#4055);
#3393=AXIS2_PLACEMENT_3D('',#5264,#4056,#4057);
#3394=AXIS2_PLACEMENT_3D('',#5265,#4058,#4059);
#3395=AXIS2_PLACEMENT_3D('',#5266,#4060,#4061);
#3396=AXIS2_PLACEMENT_3D('',#5267,#4062,#4063);
#3397=AXIS2_PLACEMENT_3D('',#5268,#4064,#4065);
#3398=AXIS2_PLACEMENT_3D('',#5269,#4066,#4067);
#3399=AXIS2_PLACEMENT_3D('',#5271,#4068,#4069);
#3400=AXIS2_PLACEMENT_3D('',#5274,#4071,#4072);
#3401=AXIS2_PLACEMENT_3D('',#5275,#4073,#4074);
#3402=AXIS2_PLACEMENT_3D('',#5277,#4075,#4076);
#3403=AXIS2_PLACEMENT_3D('',#5280,#4078,#4079);
#3404=AXIS2_PLACEMENT_3D('',#5281,#4080,#4081);
#3405=AXIS2_PLACEMENT_3D('',#5283,#4082,#4083);
#3406=AXIS2_PLACEMENT_3D('',#5286,#4085,#4086);
#3407=AXIS2_PLACEMENT_3D('',#5287,#4087,#4088);
#3408=AXIS2_PLACEMENT_3D('',#5289,#4089,#4090);
#3409=AXIS2_PLACEMENT_3D('',#5292,#4092,#4093);
#3410=AXIS2_PLACEMENT_3D('',#5293,#4094,#4095);
#3411=AXIS2_PLACEMENT_3D('',#5295,#4096,#4097);
#3412=AXIS2_PLACEMENT_3D('',#5298,#4099,#4100);
#3413=AXIS2_PLACEMENT_3D('',#5299,#4101,#4102);
#3414=AXIS2_PLACEMENT_3D('',#5301,#4103,#4104);
#3415=AXIS2_PLACEMENT_3D('',#5304,#4106,#4107);
#3416=AXIS2_PLACEMENT_3D('',#5305,#4108,#4109);
#3417=AXIS2_PLACEMENT_3D('',#5307,#4110,#4111);
#3418=AXIS2_PLACEMENT_3D('',#5310,#4113,#4114);
#3419=AXIS2_PLACEMENT_3D('',#5311,#4115,#4116);
#3420=AXIS2_PLACEMENT_3D('',#5313,#4117,#4118);
#3421=AXIS2_PLACEMENT_3D('',#5316,#4120,#4121);
#3422=AXIS2_PLACEMENT_3D('',#5317,#4122,#4123);
#3423=AXIS2_PLACEMENT_3D('',#5334,#4132,#4133);
#3424=AXIS2_PLACEMENT_3D('',#5351,#4142,#4143);
#3425=AXIS2_PLACEMENT_3D('',#5354,#4146,#4147);
#3426=AXIS2_PLACEMENT_3D('',#5356,#4149,#4150);
#3427=AXIS2_PLACEMENT_3D('',#5358,#4152,#4153);
#3428=AXIS2_PLACEMENT_3D('',#5359,#4154,#4155);
#3429=AXIS2_PLACEMENT_3D('',#5362,#4158,#4159);
#3430=AXIS2_PLACEMENT_3D('',#5364,#4161,#4162);
#3431=AXIS2_PLACEMENT_3D('',#5366,#4164,#4165);
#3432=AXIS2_PLACEMENT_3D('',#5367,#4166,#4167);
#3433=AXIS2_PLACEMENT_3D('',#5368,#4168,#4169);
#3434=AXIS2_PLACEMENT_3D('',#5371,#4170,#4171);
#3435=AXIS2_PLACEMENT_3D('',#5372,#4172,#4173);
#3436=AXIS2_PLACEMENT_3D('',#5375,#4175,#4176);
#3437=AXIS2_PLACEMENT_3D('',#5376,#4177,#4178);
#3438=AXIS2_PLACEMENT_3D('',#5379,#4179,#4180);
#3439=AXIS2_PLACEMENT_3D('',#5380,#4181,#4182);
#3440=AXIS2_PLACEMENT_3D('',#5383,#4184,#4185);
#3441=AXIS2_PLACEMENT_3D('',#5384,#4186,#4187);
#3442=AXIS2_PLACEMENT_3D('',#5386,#4188,#4189);
#3443=AXIS2_PLACEMENT_3D('',#5389,#4191,#4192);
#3444=AXIS2_PLACEMENT_3D('',#5390,#4193,#4194);
#3445=AXIS2_PLACEMENT_3D('',#5392,#4195,#4196);
#3446=AXIS2_PLACEMENT_3D('',#5395,#4198,#4199);
#3447=AXIS2_PLACEMENT_3D('',#5396,#4200,#4201);
#3448=AXIS2_PLACEMENT_3D('',#5398,#4203,#4204);
#3449=AXIS2_PLACEMENT_3D('',#5400,#4205,#4206);
#3450=AXIS2_PLACEMENT_3D('',#5402,#4208,#4209);
#3451=AXIS2_PLACEMENT_3D('',#5405,#4211,#4212);
#3452=AXIS2_PLACEMENT_3D('',#5406,#4213,#4214);
#3453=AXIS2_PLACEMENT_3D('',#5407,#4215,#4216);
#3454=AXIS2_PLACEMENT_3D('',#5408,#4217,#4218);
#3455=AXIS2_PLACEMENT_3D('',#5409,#4219,#4220);
#3456=AXIS2_PLACEMENT_3D('',#5410,#4221,#4222);
#3457=AXIS2_PLACEMENT_3D('',#5411,#4223,#4224);
#3458=AXIS2_PLACEMENT_3D('',#5416,#4226,#4227);
#3459=AXIS2_PLACEMENT_3D('',#5418,#4228,#4229);
#3460=AXIS2_PLACEMENT_3D('',#5420,#4230,#4231);
#3461=AXIS2_PLACEMENT_3D('',#5422,#4232,#4233);
#3462=AXIS2_PLACEMENT_3D('',#5424,#4234,#4235);
#3463=AXIS2_PLACEMENT_3D('',#5425,#4236,#4237);
#3464=AXIS2_PLACEMENT_3D('',#5426,#4238,#4239);
#3465=AXIS2_PLACEMENT_3D('',#5429,#4240,#4241);
#3466=AXIS2_PLACEMENT_3D('',#5430,#4242,#4243);
#3467=AXIS2_PLACEMENT_3D('',#5432,#4244,#4245);
#3468=AXIS2_PLACEMENT_3D('',#5433,#4246,#4247);
#3469=AXIS2_PLACEMENT_3D('',#5434,#4248,#4249);
#3470=AXIS2_PLACEMENT_3D('',#5437,#4250,#4251);
#3471=AXIS2_PLACEMENT_3D('',#5440,#4253,#4254);
#3472=AXIS2_PLACEMENT_3D('',#5441,#4255,#4256);
#3473=AXIS2_PLACEMENT_3D('',#5442,#4257,#4258);
#3474=AXIS2_PLACEMENT_3D('',#5445,#4260,#4261);
#3475=AXIS2_PLACEMENT_3D('',#5446,#4262,#4263);
#3476=AXIS2_PLACEMENT_3D('',#5449,#4265,#4266);
#3477=AXIS2_PLACEMENT_3D('',#5450,#4267,#4268);
#3478=AXIS2_PLACEMENT_3D('',#5453,#4270,#4271);
#3479=AXIS2_PLACEMENT_3D('',#5454,#4272,#4273);
#3480=AXIS2_PLACEMENT_3D('',#5467,#4280,#4281);
#3481=AXIS2_PLACEMENT_3D('',#5468,#4282,#4283);
#3482=AXIS2_PLACEMENT_3D('',#5469,#4284,#4285);
#3483=AXIS2_PLACEMENT_3D('',#5476,#4290,#4291);
#3484=AXIS2_PLACEMENT_3D('',#5481,#4295,#4296);
#3485=AXIS2_PLACEMENT_3D('',#5486,#4300,#4301);
#3486=AXIS2_PLACEMENT_3D('',#5491,#4305,#4306);
#3487=AXIS2_PLACEMENT_3D('',#5496,#4310,#4311);
#3488=AXIS2_PLACEMENT_3D('',#5499,#4314,#4315);
#3489=AXIS2_PLACEMENT_3D('',#5500,#4316,#4317);
#3490=AXIS2_PLACEMENT_3D('',#5501,#4318,#4319);
#3491=AXIS2_PLACEMENT_3D('',#5502,#4320,#4321);
#3492=AXIS2_PLACEMENT_3D('',#5503,#4322,#4323);
#3493=AXIS2_PLACEMENT_3D('',#5504,#4324,#4325);
#3494=AXIS2_PLACEMENT_3D('',#5505,#4326,#4327);
#3495=AXIS2_PLACEMENT_3D('',#5506,#4328,#4329);
#3496=AXIS2_PLACEMENT_3D('',#5508,#4330,#4331);
#3497=AXIS2_PLACEMENT_3D('',#5511,#4333,#4334);
#3498=AXIS2_PLACEMENT_3D('',#5512,#4335,#4336);
#3499=AXIS2_PLACEMENT_3D('',#5514,#4337,#4338);
#3500=AXIS2_PLACEMENT_3D('',#5517,#4340,#4341);
#3501=AXIS2_PLACEMENT_3D('',#5518,#4342,#4343);
#3502=AXIS2_PLACEMENT_3D('',#5519,#4344,#4345);
#3503=AXIS2_PLACEMENT_3D('',#5520,#4346,#4347);
#3504=AXIS2_PLACEMENT_3D('',#5521,#4348,#4349);
#3505=AXIS2_PLACEMENT_3D('',#5526,#4351,#4352);
#3506=AXIS2_PLACEMENT_3D('',#5528,#4353,#4354);
#3507=AXIS2_PLACEMENT_3D('',#5530,#4355,#4356);
#3508=AXIS2_PLACEMENT_3D('',#5532,#4357,#4358);
#3509=AXIS2_PLACEMENT_3D('',#5534,#4359,#4360);
#3510=AXIS2_PLACEMENT_3D('',#5535,#4361,#4362);
#3511=AXIS2_PLACEMENT_3D('',#5536,#4363,#4364);
#3512=AXIS2_PLACEMENT_3D('',#5539,#4365,#4366);
#3513=AXIS2_PLACEMENT_3D('',#5540,#4367,#4368);
#3514=AXIS2_PLACEMENT_3D('',#5542,#4369,#4370);
#3515=AXIS2_PLACEMENT_3D('',#5543,#4371,#4372);
#3516=AXIS2_PLACEMENT_3D('',#5544,#4373,#4374);
#3517=AXIS2_PLACEMENT_3D('',#5546,#4375,#4376);
#3518=AXIS2_PLACEMENT_3D('',#5549,#4378,#4379);
#3519=AXIS2_PLACEMENT_3D('',#5550,#4380,#4381);
#3520=AXIS2_PLACEMENT_3D('',#5552,#4383,#4384);
#3521=AXIS2_PLACEMENT_3D('',#5555,#4385,#4386);
#3522=AXIS2_PLACEMENT_3D('',#5556,#4387,#4388);
#3523=AXIS2_PLACEMENT_3D('',#5559,#4390,#4391);
#3524=AXIS2_PLACEMENT_3D('',#5560,#4392,#4393);
#3525=AXIS2_PLACEMENT_3D('',#5563,#4395,#4396);
#3526=AXIS2_PLACEMENT_3D('',#5564,#4397,#4398);
#3527=AXIS2_PLACEMENT_3D('',#5577,#4405,#4406);
#3528=AXIS2_PLACEMENT_3D('',#5578,#4407,#4408);
#3529=AXIS2_PLACEMENT_3D('',#5579,#4409,#4410);
#3530=AXIS2_PLACEMENT_3D('',#5586,#4415,#4416);
#3531=AXIS2_PLACEMENT_3D('',#5591,#4420,#4421);
#3532=AXIS2_PLACEMENT_3D('',#5596,#4425,#4426);
#3533=AXIS2_PLACEMENT_3D('',#5601,#4430,#4431);
#3534=AXIS2_PLACEMENT_3D('',#5606,#4435,#4436);
#3535=AXIS2_PLACEMENT_3D('',#5609,#4439,#4440);
#3536=AXIS2_PLACEMENT_3D('',#5610,#4441,#4442);
#3537=AXIS2_PLACEMENT_3D('',#5611,#4443,#4444);
#3538=AXIS2_PLACEMENT_3D('',#5612,#4445,#4446);
#3539=AXIS2_PLACEMENT_3D('',#5613,#4447,#4448);
#3540=AXIS2_PLACEMENT_3D('',#5614,#4449,#4450);
#3541=AXIS2_PLACEMENT_3D('',#5615,#4451,#4452);
#3542=AXIS2_PLACEMENT_3D('',#5616,#4453,#4454);
#3543=AXIS2_PLACEMENT_3D('',#5617,#4455,#4456);
#3544=AXIS2_PLACEMENT_3D('',#5618,#4457,#4458);
#3545=AXIS2_PLACEMENT_3D('',#5619,#4459,#4460);
#3546=AXIS2_PLACEMENT_3D('',#5620,#4461,#4462);
#3547=AXIS2_PLACEMENT_3D('',#5621,#4463,#4464);
#3548=AXIS2_PLACEMENT_3D('',#5622,#4465,#4466);
#3549=AXIS2_PLACEMENT_3D('',#5623,#4467,#4468);
#3550=AXIS2_PLACEMENT_3D('',#5624,#4469,#4470);
#3551=AXIS2_PLACEMENT_3D('',#5625,#4471,#4472);
#3552=AXIS2_PLACEMENT_3D('',#5626,#4473,#4474);
#3553=AXIS2_PLACEMENT_3D('',#5627,#4475,#4476);
#3554=AXIS2_PLACEMENT_3D('',#5628,#4477,#4478);
#3555=AXIS2_PLACEMENT_3D('',#5629,#4479,#4480);
#3556=AXIS2_PLACEMENT_3D('',#5630,#4481,#4482);
#3557=AXIS2_PLACEMENT_3D('',#5631,#4483,#4484);
#3558=AXIS2_PLACEMENT_3D('',#5632,#4485,#4486);
#3559=DIRECTION('axis',(0.,0.,1.));
#3560=DIRECTION('refdir',(1.,0.,0.));
#3561=DIRECTION('axis',(0.,0.,1.));
#3562=DIRECTION('refdir',(1.,0.,0.));
#3563=DIRECTION('center_axis',(1.,0.,0.));
#3564=DIRECTION('ref_axis',(0.,0.,-1.));
#3565=DIRECTION('center_axis',(1.,0.,0.));
#3566=DIRECTION('ref_axis',(0.,1.,0.));
#3567=DIRECTION('',(0.,1.,1.79594901042305E-16));
#3568=DIRECTION('center_axis',(1.,0.,0.));
#3569=DIRECTION('ref_axis',(0.,1.,0.));
#3570=DIRECTION('',(0.,-1.,-1.79594901042305E-16));
#3571=DIRECTION('',(0.,1.,1.79594901042305E-16));
#3572=DIRECTION('center_axis',(1.,0.,0.));
#3573=DIRECTION('ref_axis',(0.,0.,-1.));
#3574=DIRECTION('',(0.,-1.,-1.79594901042305E-16));
#3575=DIRECTION('center_axis',(1.,0.,0.));
#3576=DIRECTION('ref_axis',(0.,0.,-1.));
#3577=DIRECTION('center_axis',(1.,0.,0.));
#3578=DIRECTION('ref_axis',(0.,0.,-1.));
#3579=DIRECTION('center_axis',(1.,0.,0.));
#3580=DIRECTION('ref_axis',(0.,1.,0.));
#3581=DIRECTION('',(0.,-1.,-1.79594901042305E-16));
#3582=DIRECTION('center_axis',(1.,0.,0.));
#3583=DIRECTION('ref_axis',(0.,1.,0.));
#3584=DIRECTION('',(0.,1.,1.79594901042305E-16));
#3585=DIRECTION('center_axis',(1.,0.,0.));
#3586=DIRECTION('ref_axis',(0.,0.,-1.));
#3587=DIRECTION('',(0.,1.,1.79594901042305E-16));
#3588=DIRECTION('center_axis',(1.,0.,0.));
#3589=DIRECTION('ref_axis',(0.,0.,-1.));
#3590=DIRECTION('',(0.,-1.,-1.79594901042305E-16));
#3591=DIRECTION('center_axis',(-1.,0.,0.));
#3592=DIRECTION('ref_axis',(0.,0.,1.));
#3593=DIRECTION('',(-1.,0.,0.));
#3594=DIRECTION('',(-1.,0.,0.));
#3595=DIRECTION('center_axis',(0.,-1.79594901042305E-16,1.));
#3596=DIRECTION('ref_axis',(0.,-1.,-1.79594901042305E-16));
#3597=DIRECTION('',(-1.,0.,0.));
#3598=DIRECTION('center_axis',(-1.,0.,0.));
#3599=DIRECTION('ref_axis',(0.,0.,1.));
#3600=DIRECTION('',(-1.,0.,0.));
#3601=DIRECTION('center_axis',(0.,1.79594901042305E-16,-1.));
#3602=DIRECTION('ref_axis',(0.,1.,1.79594901042305E-16));
#3603=DIRECTION('center_axis',(-1.,0.,0.));
#3604=DIRECTION('ref_axis',(0.,0.,1.));
#3605=DIRECTION('',(-1.,0.,0.));
#3606=DIRECTION('',(-1.,0.,0.));
#3607=DIRECTION('center_axis',(0.,-1.79594901042305E-16,1.));
#3608=DIRECTION('ref_axis',(0.,-1.,-1.79594901042305E-16));
#3609=DIRECTION('',(-1.,0.,0.));
#3610=DIRECTION('center_axis',(-1.,0.,0.));
#3611=DIRECTION('ref_axis',(0.,0.,1.));
#3612=DIRECTION('',(-1.,0.,0.));
#3613=DIRECTION('center_axis',(0.,1.79594901042305E-16,-1.));
#3614=DIRECTION('ref_axis',(0.,1.,1.79594901042305E-16));
#3615=DIRECTION('axis',(0.,0.,1.));
#3616=DIRECTION('refdir',(1.,0.,0.));
#3617=DIRECTION('center_axis',(0.,0.,-1.));
#3618=DIRECTION('ref_axis',(-1.,0.,0.));
#3619=DIRECTION('center_axis',(0.,0.,1.));
#3620=DIRECTION('ref_axis',(1.,0.,0.));
#3621=DIRECTION('',(0.,0.,-1.));
#3622=DIRECTION('center_axis',(0.,0.,1.));
#3623=DIRECTION('ref_axis',(1.,0.,0.));
#3624=DIRECTION('center_axis',(0.,0.,-1.));
#3625=DIRECTION('ref_axis',(-1.,0.,0.));
#3626=DIRECTION('center_axis',(0.,0.,1.));
#3627=DIRECTION('ref_axis',(1.,0.,0.));
#3628=DIRECTION('',(0.,0.,-1.));
#3629=DIRECTION('center_axis',(0.,0.,1.));
#3630=DIRECTION('ref_axis',(1.,0.,0.));
#3631=DIRECTION('center_axis',(0.,0.,-1.));
#3632=DIRECTION('ref_axis',(-1.,0.,0.));
#3633=DIRECTION('center_axis',(0.,0.,1.));
#3634=DIRECTION('ref_axis',(1.,0.,0.));
#3635=DIRECTION('',(0.,0.,-1.));
#3636=DIRECTION('center_axis',(0.,0.,1.));
#3637=DIRECTION('ref_axis',(1.,0.,0.));
#3638=DIRECTION('center_axis',(0.,0.,-1.));
#3639=DIRECTION('ref_axis',(-1.,0.,0.));
#3640=DIRECTION('center_axis',(0.,0.,1.));
#3641=DIRECTION('ref_axis',(1.,0.,0.));
#3642=DIRECTION('',(0.,0.,-1.));
#3643=DIRECTION('center_axis',(0.,0.,1.));
#3644=DIRECTION('ref_axis',(1.,0.,0.));
#3645=DIRECTION('center_axis',(0.,0.,-1.));
#3646=DIRECTION('ref_axis',(-1.,0.,0.));
#3647=DIRECTION('center_axis',(0.,0.,1.));
#3648=DIRECTION('ref_axis',(1.,0.,0.));
#3649=DIRECTION('',(0.,0.,-1.));
#3650=DIRECTION('center_axis',(0.,0.,1.));
#3651=DIRECTION('ref_axis',(1.,0.,0.));
#3652=DIRECTION('center_axis',(0.,0.,-1.));
#3653=DIRECTION('ref_axis',(-1.,0.,0.));
#3654=DIRECTION('center_axis',(0.,0.,1.));
#3655=DIRECTION('ref_axis',(1.,0.,0.));
#3656=DIRECTION('',(0.,0.,-1.));
#3657=DIRECTION('center_axis',(0.,0.,1.));
#3658=DIRECTION('ref_axis',(1.,0.,0.));
#3659=DIRECTION('center_axis',(0.,0.,1.));
#3660=DIRECTION('ref_axis',(1.,0.,0.));
#3661=DIRECTION('',(1.,0.,0.));
#3662=DIRECTION('',(7.22801448323673E-16,1.,0.));
#3663=DIRECTION('center_axis',(0.,0.,1.));
#3664=DIRECTION('ref_axis',(1.,0.,0.));
#3665=DIRECTION('',(1.15648231731788E-15,-1.,0.));
#3666=DIRECTION('center_axis',(0.,0.,1.));
#3667=DIRECTION('ref_axis',(1.,0.,0.));
#3668=DIRECTION('',(1.,0.,0.));
#3669=DIRECTION('',(1.15648231731788E-15,-1.,0.));
#3670=DIRECTION('center_axis',(0.,0.,1.));
#3671=DIRECTION('ref_axis',(1.,0.,0.));
#3672=DIRECTION('',(7.22801448323673E-16,1.,0.));
#3673=DIRECTION('center_axis',(0.,1.,0.));
#3674=DIRECTION('ref_axis',(0.,0.,1.));
#3675=DIRECTION('',(0.,0.,-1.));
#3676=DIRECTION('',(0.,0.,-1.));
#3677=DIRECTION('center_axis',(-1.,7.22801448323673E-16,0.));
#3678=DIRECTION('ref_axis',(-7.22801448323673E-16,-1.,0.));
#3679=DIRECTION('',(0.,0.,-1.));
#3680=DIRECTION('center_axis',(0.,0.,-1.));
#3681=DIRECTION('ref_axis',(-1.,0.,0.));
#3682=DIRECTION('',(0.,0.,-1.));
#3683=DIRECTION('center_axis',(1.,1.15648231731788E-15,0.));
#3684=DIRECTION('ref_axis',(-1.15648231731788E-15,1.,0.));
#3685=DIRECTION('axis',(0.,0.,1.));
#3686=DIRECTION('refdir',(1.,0.,0.));
#3687=DIRECTION('center_axis',(-1.,0.,0.));
#3688=DIRECTION('ref_axis',(0.,0.,1.));
#3689=DIRECTION('center_axis',(0.,-1.,0.));
#3690=DIRECTION('ref_axis',(0.,0.,1.));
#3691=DIRECTION('center_axis',(-1.,0.,0.));
#3692=DIRECTION('ref_axis',(0.,0.,1.));
#3693=DIRECTION('center_axis',(0.,-6.12323399573677E-17,1.));
#3694=DIRECTION('ref_axis',(0.,-1.,-6.12323399573677E-17));
#3695=DIRECTION('center_axis',(-1.,0.,0.));
#3696=DIRECTION('ref_axis',(0.,0.,1.));
#3697=DIRECTION('center_axis',(0.,0.,1.));
#3698=DIRECTION('ref_axis',(1.,0.,0.));
#3699=DIRECTION('center_axis',(1.,0.,0.));
#3700=DIRECTION('ref_axis',(0.,0.,1.));
#3701=DIRECTION('center_axis',(0.,-1.,4.68844182696434E-17));
#3702=DIRECTION('ref_axis',(1.,0.,0.));
#3703=DIRECTION('center_axis',(1.,0.,0.));
#3704=DIRECTION('ref_axis',(0.,0.,-1.));
#3705=DIRECTION('',(1.,0.,0.));
#3706=DIRECTION('center_axis',(1.,0.,0.));
#3707=DIRECTION('ref_axis',(0.,0.,-1.));
#3708=DIRECTION('',(1.,0.,0.));
#3709=DIRECTION('center_axis',(0.,0.,-1.));
#3710=DIRECTION('ref_axis',(-1.,0.,0.));
#3711=DIRECTION('center_axis',(0.,0.,1.));
#3712=DIRECTION('ref_axis',(1.,0.,0.));
#3713=DIRECTION('',(0.,0.,-1.));
#3714=DIRECTION('center_axis',(0.,0.,1.));
#3715=DIRECTION('ref_axis',(1.,0.,0.));
#3716=DIRECTION('center_axis',(0.,0.,-1.));
#3717=DIRECTION('ref_axis',(-1.,0.,0.));
#3718=DIRECTION('center_axis',(0.,0.,1.));
#3719=DIRECTION('ref_axis',(1.,0.,0.));
#3720=DIRECTION('',(0.,0.,-1.));
#3721=DIRECTION('center_axis',(0.,0.,1.));
#3722=DIRECTION('ref_axis',(1.,0.,0.));
#3723=DIRECTION('center_axis',(0.,0.,-1.));
#3724=DIRECTION('ref_axis',(-1.,0.,0.));
#3725=DIRECTION('center_axis',(0.,0.,1.));
#3726=DIRECTION('ref_axis',(1.,0.,0.));
#3727=DIRECTION('',(0.,0.,-1.));
#3728=DIRECTION('center_axis',(0.,0.,1.));
#3729=DIRECTION('ref_axis',(1.,0.,0.));
#3730=DIRECTION('center_axis',(0.,0.,-1.));
#3731=DIRECTION('ref_axis',(-1.,0.,0.));
#3732=DIRECTION('center_axis',(0.,0.,1.));
#3733=DIRECTION('ref_axis',(1.,0.,0.));
#3734=DIRECTION('',(0.,0.,-1.));
#3735=DIRECTION('center_axis',(0.,0.,1.));
#3736=DIRECTION('ref_axis',(1.,0.,0.));
#3737=DIRECTION('center_axis',(0.,0.,-1.));
#3738=DIRECTION('ref_axis',(-1.,0.,0.));
#3739=DIRECTION('center_axis',(0.,0.,1.));
#3740=DIRECTION('ref_axis',(1.,0.,0.));
#3741=DIRECTION('',(0.,0.,1.));
#3742=DIRECTION('center_axis',(0.,0.,1.));
#3743=DIRECTION('ref_axis',(1.,0.,0.));
#3744=DIRECTION('center_axis',(0.,4.68844182696434E-17,-1.));
#3745=DIRECTION('ref_axis',(0.,1.,4.68844182696434E-17));
#3746=DIRECTION('',(0.,4.68844182696434E-17,-1.));
#3747=DIRECTION('center_axis',(0.,0.,1.));
#3748=DIRECTION('ref_axis',(1.,0.,0.));
#3749=DIRECTION('center_axis',(0.,1.,0.));
#3750=DIRECTION('ref_axis',(0.,0.,1.));
#3751=DIRECTION('center_axis',(0.,-1.,4.68844182696434E-17));
#3752=DIRECTION('ref_axis',(0.,-4.68844182696434E-17,-1.));
#3753=DIRECTION('',(0.,1.,0.));
#3754=DIRECTION('center_axis',(0.,4.68844182696434E-17,-1.));
#3755=DIRECTION('ref_axis',(0.,1.,4.68844182696434E-17));
#3756=DIRECTION('center_axis',(0.,0.,1.));
#3757=DIRECTION('ref_axis',(1.,0.,0.));
#3758=DIRECTION('',(0.,-4.68844182696434E-17,1.));
#3759=DIRECTION('center_axis',(0.,1.,0.));
#3760=DIRECTION('ref_axis',(0.,0.,1.));
#3761=DIRECTION('',(0.,-1.,0.));
#3762=DIRECTION('center_axis',(0.,-1.,4.68844182696434E-17));
#3763=DIRECTION('ref_axis',(1.,0.,0.));
#3764=DIRECTION('center_axis',(0.,-1.,4.68844182696434E-17));
#3765=DIRECTION('ref_axis',(1.,0.,0.));
#3766=DIRECTION('center_axis',(0.,0.,1.));
#3767=DIRECTION('ref_axis',(1.,0.,0.));
#3768=DIRECTION('center_axis',(0.,0.,1.));
#3769=DIRECTION('ref_axis',(1.,0.,0.));
#3770=DIRECTION('center_axis',(0.,0.,1.));
#3771=DIRECTION('ref_axis',(1.,0.,0.));
#3772=DIRECTION('axis',(0.,0.,1.));
#3773=DIRECTION('refdir',(1.,0.,0.));
#3774=DIRECTION('center_axis',(0.,1.,0.));
#3775=DIRECTION('ref_axis',(0.,0.,1.));
#3776=DIRECTION('center_axis',(0.,1.,0.));
#3777=DIRECTION('ref_axis',(0.,0.,1.));
#3778=DIRECTION('',(0.,1.,0.));
#3779=DIRECTION('center_axis',(0.,1.,0.));
#3780=DIRECTION('ref_axis',(0.,0.,1.));
#3781=DIRECTION('center_axis',(0.,1.,0.));
#3782=DIRECTION('ref_axis',(0.,0.,1.));
#3783=DIRECTION('center_axis',(0.,1.,0.));
#3784=DIRECTION('ref_axis',(0.,0.,1.));
#3785=DIRECTION('',(0.,1.,0.));
#3786=DIRECTION('center_axis',(0.,1.,0.));
#3787=DIRECTION('ref_axis',(0.,0.,1.));
#3788=DIRECTION('center_axis',(-1.,0.,-7.76407098792971E-16));
#3789=DIRECTION('ref_axis',(-7.76407098792971E-16,0.,1.));
#3790=DIRECTION('center_axis',(-1.,0.,-7.76407098792971E-16));
#3791=DIRECTION('ref_axis',(-7.76407098792971E-16,0.,1.));
#3792=DIRECTION('',(1.,0.,7.76407098792971E-16));
#3793=DIRECTION('center_axis',(-1.,0.,-7.76407098792971E-16));
#3794=DIRECTION('ref_axis',(-7.76407098792971E-16,0.,1.));
#3795=DIRECTION('center_axis',(-1.,0.,-7.76407098792971E-16));
#3796=DIRECTION('ref_axis',(-7.76407098792971E-16,0.,1.));
#3797=DIRECTION('center_axis',(-9.50824468372095E-32,-1.,1.22464679914735E-16));
#3798=DIRECTION('ref_axis',(7.73103237808434E-16,-1.22464679914735E-16,
-1.));
#3799=DIRECTION('center_axis',(-1.,0.,-7.76407098792971E-16));
#3800=DIRECTION('ref_axis',(-7.76407098792971E-16,0.,1.));
#3801=DIRECTION('center_axis',(-1.,0.,-7.76407098792971E-16));
#3802=DIRECTION('ref_axis',(-7.76407098792971E-16,0.,1.));
#3803=DIRECTION('',(-1.,0.,-7.76407098792971E-16));
#3804=DIRECTION('center_axis',(0.,-1.,0.));
#3805=DIRECTION('ref_axis',(0.,0.,-1.));
#3806=DIRECTION('center_axis',(0.,1.,0.));
#3807=DIRECTION('ref_axis',(0.,0.,1.));
#3808=DIRECTION('',(0.,-1.,0.));
#3809=DIRECTION('center_axis',(0.,1.,0.));
#3810=DIRECTION('ref_axis',(0.,0.,1.));
#3811=DIRECTION('',(0.,-1.,0.));
#3812=DIRECTION('center_axis',(0.295992012371146,0.,-0.955190414845375));
#3813=DIRECTION('ref_axis',(-0.955190414845375,0.,-0.295992012371146));
#3814=DIRECTION('',(0.955190414845375,0.,0.295992012371146));
#3815=DIRECTION('',(0.955190414845375,0.,0.295992012371146));
#3816=DIRECTION('',(0.,-1.,0.));
#3817=DIRECTION('center_axis',(0.295992012371146,0.,0.955190414845375));
#3818=DIRECTION('ref_axis',(0.955190414845375,0.,-0.295992012371146));
#3819=DIRECTION('',(-0.955190414845375,0.,0.295992012371146));
#3820=DIRECTION('',(0.,-1.,0.));
#3821=DIRECTION('',(-0.955190414845375,0.,0.295992012371146));
#3822=DIRECTION('center_axis',(1.,0.,0.));
#3823=DIRECTION('ref_axis',(0.,0.,-1.));
#3824=DIRECTION('center_axis',(1.,0.,0.));
#3825=DIRECTION('ref_axis',(0.,0.,1.));
#3826=DIRECTION('',(1.,0.,0.));
#3827=DIRECTION('center_axis',(1.,0.,0.));
#3828=DIRECTION('ref_axis',(0.,0.,1.));
#3829=DIRECTION('',(1.,0.,0.));
#3830=DIRECTION('center_axis',(0.,-1.,0.));
#3831=DIRECTION('ref_axis',(0.,0.,-1.));
#3832=DIRECTION('',(0.,0.,-1.));
#3833=DIRECTION('',(1.,0.,0.));
#3834=DIRECTION('',(0.,0.,-1.));
#3835=DIRECTION('center_axis',(1.,0.,0.));
#3836=DIRECTION('ref_axis',(0.,0.,-1.));
#3837=DIRECTION('center_axis',(1.,0.,0.));
#3838=DIRECTION('ref_axis',(0.,0.,1.));
#3839=DIRECTION('',(1.,0.,0.));
#3840=DIRECTION('center_axis',(1.,0.,0.));
#3841=DIRECTION('ref_axis',(0.,0.,1.));
#3842=DIRECTION('center_axis',(0.,8.67361737988404E-17,1.));
#3843=DIRECTION('ref_axis',(0.,-1.,8.67361737988404E-17));
#3844=DIRECTION('',(0.,-1.,8.67361737988404E-17));
#3845=DIRECTION('',(1.,0.,0.));
#3846=DIRECTION('',(0.,-1.,8.67361737988404E-17));
#3847=DIRECTION('center_axis',(1.,0.,0.));
#3848=DIRECTION('ref_axis',(0.,0.,-1.));
#3849=DIRECTION('center_axis',(1.,0.,0.));
#3850=DIRECTION('ref_axis',(0.,0.,1.));
#3851=DIRECTION('',(1.,0.,0.));
#3852=DIRECTION('center_axis',(1.,0.,0.));
#3853=DIRECTION('ref_axis',(0.,0.,1.));
#3854=DIRECTION('center_axis',(0.,1.,0.));
#3855=DIRECTION('ref_axis',(0.,0.,1.));
#3856=DIRECTION('',(0.,0.,1.));
#3857=DIRECTION('',(1.,0.,0.));
#3858=DIRECTION('',(0.,0.,1.));
#3859=DIRECTION('center_axis',(1.,0.,0.));
#3860=DIRECTION('ref_axis',(0.,0.,-1.));
#3861=DIRECTION('center_axis',(1.,0.,0.));
#3862=DIRECTION('ref_axis',(0.,0.,-1.));
#3863=DIRECTION('',(1.,0.,0.));
#3864=DIRECTION('center_axis',(1.,0.,0.));
#3865=DIRECTION('ref_axis',(0.,0.,-1.));
#3866=DIRECTION('center_axis',(0.,-8.67361737988404E-17,-1.));
#3867=DIRECTION('ref_axis',(0.,1.,-8.67361737988404E-17));
#3868=DIRECTION('',(0.,1.,-8.67361737988404E-17));
#3869=DIRECTION('',(0.,1.,-8.67361737988404E-17));
#3870=DIRECTION('center_axis',(-1.,0.,0.));
#3871=DIRECTION('ref_axis',(0.,0.,1.));
#3872=DIRECTION('',(0.,-1.,0.));
#3873=DIRECTION('',(0.,0.,-1.));
#3874=DIRECTION('',(0.,-1.,0.));
#3875=DIRECTION('',(0.,0.,-1.));
#3876=DIRECTION('',(0.,0.,-1.));
#3877=DIRECTION('',(0.,0.,-1.));
#3878=DIRECTION('center_axis',(-1.,0.,0.));
#3879=DIRECTION('ref_axis',(0.,0.,1.));
#3880=DIRECTION('center_axis',(-1.,0.,-7.76407098792971E-16));
#3881=DIRECTION('ref_axis',(-7.76407098792971E-16,0.,1.));
#3882=DIRECTION('center_axis',(0.,-1.,0.));
#3883=DIRECTION('ref_axis',(0.,0.,-1.));
#3884=DIRECTION('',(0.,-1.,0.));
#3885=DIRECTION('center_axis',(0.,1.,0.));
#3886=DIRECTION('ref_axis',(0.,0.,1.));
#3887=DIRECTION('',(0.,-1.,0.));
#3888=DIRECTION('center_axis',(0.,1.,0.));
#3889=DIRECTION('ref_axis',(0.,0.,1.));
#3890=DIRECTION('center_axis',(0.295992012371146,0.,-0.955190414845375));
#3891=DIRECTION('ref_axis',(-0.955190414845375,0.,-0.295992012371146));
#3892=DIRECTION('',(0.955190414845375,0.,0.295992012371146));
#3893=DIRECTION('',(0.955190414845375,0.,0.295992012371146));
#3894=DIRECTION('center_axis',(0.295992012371146,0.,0.955190414845375));
#3895=DIRECTION('ref_axis',(0.955190414845375,0.,-0.295992012371146));
#3896=DIRECTION('',(-0.955190414845375,0.,0.295992012371146));
#3897=DIRECTION('',(-0.955190414845375,0.,0.295992012371146));
#3898=DIRECTION('center_axis',(0.,1.,0.));
#3899=DIRECTION('ref_axis',(0.,0.,1.));
#3900=DIRECTION('center_axis',(0.,1.,0.));
#3901=DIRECTION('ref_axis',(0.,0.,1.));
#3902=DIRECTION('center_axis',(0.,1.,0.));
#3903=DIRECTION('ref_axis',(0.,0.,1.));
#3904=DIRECTION('center_axis',(0.,1.,0.));
#3905=DIRECTION('ref_axis',(0.,0.,1.));
#3906=DIRECTION('axis',(0.,0.,1.));
#3907=DIRECTION('refdir',(1.,0.,0.));
#3908=DIRECTION('center_axis',(0.,0.,1.));
#3909=DIRECTION('ref_axis',(1.,0.,0.));
#3910=DIRECTION('center_axis',(0.,0.,1.));
#3911=DIRECTION('ref_axis',(-1.,0.,0.));
#3912=DIRECTION('',(0.,0.,1.));
#3913=DIRECTION('center_axis',(0.,0.,1.));
#3914=DIRECTION('ref_axis',(1.,0.,0.));
#3915=DIRECTION('center_axis',(-0.500000000000003,0.866025403784437,0.));
#3916=DIRECTION('ref_axis',(-0.866025403784437,-0.500000000000003,0.));
#3917=DIRECTION('',(0.,0.,1.));
#3918=DIRECTION('',(0.,0.,1.));
#3919=DIRECTION('center_axis',(0.500000000000004,0.866025403784437,0.));
#3920=DIRECTION('ref_axis',(-0.866025403784437,0.500000000000004,0.));
#3921=DIRECTION('',(0.,0.,1.));
#3922=DIRECTION('center_axis',(-1.,0.,0.));
#3923=DIRECTION('ref_axis',(0.,0.,1.));
#3924=DIRECTION('',(0.,0.,1.));
#3925=DIRECTION('center_axis',(0.500000000000002,-0.866025403784437,0.));
#3926=DIRECTION('ref_axis',(0.866025403784437,0.500000000000002,0.));
#3927=DIRECTION('',(0.,0.,1.));
#3928=DIRECTION('center_axis',(-0.500000000000003,-0.866025403784437,0.));
#3929=DIRECTION('ref_axis',(0.866025403784437,-0.500000000000003,0.));
#3930=DIRECTION('',(0.,0.,1.));
#3931=DIRECTION('center_axis',(-1.,0.,0.));
#3932=DIRECTION('ref_axis',(0.,0.,1.));
#3933=DIRECTION('center_axis',(0.,0.,-1.));
#3934=DIRECTION('ref_axis',(-1.,0.,0.));
#3935=DIRECTION('center_axis',(0.,0.,-1.));
#3936=DIRECTION('ref_axis',(-1.,0.,0.));
#3937=DIRECTION('center_axis',(0.,0.,-1.));
#3938=DIRECTION('ref_axis',(-1.,0.,0.));
#3939=DIRECTION('center_axis',(0.,0.,-1.));
#3940=DIRECTION('ref_axis',(-1.,0.,0.));
#3941=DIRECTION('center_axis',(0.,0.,-1.));
#3942=DIRECTION('ref_axis',(-1.,0.,0.));
#3943=DIRECTION('center_axis',(0.,0.,1.));
#3944=DIRECTION('ref_axis',(1.,0.,0.));
#3945=DIRECTION('center_axis',(0.,0.,-1.));
#3946=DIRECTION('ref_axis',(-1.,0.,0.));
#3947=DIRECTION('center_axis',(0.,0.,-1.));
#3948=DIRECTION('ref_axis',(-1.,0.,0.));
#3949=DIRECTION('center_axis',(0.,0.,1.));
#3950=DIRECTION('ref_axis',(-1.,0.,0.));
#3951=DIRECTION('center_axis',(0.,0.,1.));
#3952=DIRECTION('ref_axis',(-1.,-3.5527136788005E-15,0.));
#3953=DIRECTION('center_axis',(0.,0.,1.));
#3954=DIRECTION('ref_axis',(-1.,0.,0.));
#3955=DIRECTION('center_axis',(0.,0.,1.));
#3956=DIRECTION('ref_axis',(1.,0.,0.));
#3957=DIRECTION('center_axis',(0.,0.,1.));
#3958=DIRECTION('ref_axis',(-1.,1.77635683940025E-15,0.));
#3959=DIRECTION('center_axis',(0.,0.,1.));
#3960=DIRECTION('ref_axis',(-1.,0.,0.));
#3961=DIRECTION('center_axis',(0.,0.,1.));
#3962=DIRECTION('ref_axis',(1.,0.,0.));
#3963=DIRECTION('center_axis',(0.,0.,1.));
#3964=DIRECTION('ref_axis',(1.,0.,0.));
#3965=DIRECTION('center_axis',(0.,0.,1.));
#3966=DIRECTION('ref_axis',(1.,0.,0.));
#3967=DIRECTION('center_axis',(0.,0.,1.));
#3968=DIRECTION('ref_axis',(1.,0.,0.));
#3969=DIRECTION('center_axis',(0.,0.,1.));
#3970=DIRECTION('ref_axis',(1.,0.,0.));
#3971=DIRECTION('center_axis',(0.,0.,1.));
#3972=DIRECTION('ref_axis',(1.,0.,0.));
#3973=DIRECTION('center_axis',(0.,0.,-1.));
#3974=DIRECTION('ref_axis',(-1.,0.,0.));
#3975=DIRECTION('center_axis',(0.,0.,-1.));
#3976=DIRECTION('ref_axis',(-1.,0.,0.));
#3977=DIRECTION('center_axis',(0.,0.,-1.));
#3978=DIRECTION('ref_axis',(-1.,0.,0.));
#3979=DIRECTION('center_axis',(0.,0.,-1.));
#3980=DIRECTION('ref_axis',(-1.,0.,0.));
#3981=DIRECTION('center_axis',(0.,0.,-1.));
#3982=DIRECTION('ref_axis',(-1.,0.,0.));
#3983=DIRECTION('center_axis',(0.,0.,-1.));
#3984=DIRECTION('ref_axis',(-1.,0.,0.));
#3985=DIRECTION('axis',(0.,0.,1.));
#3986=DIRECTION('refdir',(1.,0.,0.));
#3987=DIRECTION('center_axis',(0.,0.,1.));
#3988=DIRECTION('ref_axis',(1.,0.,0.));
#3989=DIRECTION('center_axis',(0.,0.,1.));
#3990=DIRECTION('ref_axis',(-1.,0.,0.));
#3991=DIRECTION('',(0.,0.,1.));
#3992=DIRECTION('center_axis',(0.,0.,1.));
#3993=DIRECTION('ref_axis',(1.,0.,0.));
#3994=DIRECTION('center_axis',(-0.500000000000003,0.866025403784437,0.));
#3995=DIRECTION('ref_axis',(-0.866025403784437,-0.500000000000003,0.));
#3996=DIRECTION('',(0.,0.,1.));
#3997=DIRECTION('',(0.,0.,1.));
#3998=DIRECTION('center_axis',(0.500000000000004,0.866025403784437,0.));
#3999=DIRECTION('ref_axis',(-0.866025403784437,0.500000000000004,0.));
#4000=DIRECTION('',(0.,0.,1.));
#4001=DIRECTION('center_axis',(-1.,0.,0.));
#4002=DIRECTION('ref_axis',(0.,0.,1.));
#4003=DIRECTION('',(0.,0.,1.));
#4004=DIRECTION('center_axis',(0.500000000000002,-0.866025403784437,0.));
#4005=DIRECTION('ref_axis',(0.866025403784437,0.500000000000002,0.));
#4006=DIRECTION('',(0.,0.,1.));
#4007=DIRECTION('center_axis',(-0.500000000000003,-0.866025403784437,0.));
#4008=DIRECTION('ref_axis',(0.866025403784437,-0.500000000000003,0.));
#4009=DIRECTION('',(0.,0.,1.));
#4010=DIRECTION('center_axis',(-1.,0.,0.));
#4011=DIRECTION('ref_axis',(0.,0.,1.));
#4012=DIRECTION('center_axis',(0.,0.,-1.));
#4013=DIRECTION('ref_axis',(-1.,0.,0.));
#4014=DIRECTION('center_axis',(0.,0.,-1.));
#4015=DIRECTION('ref_axis',(-1.,0.,0.));
#4016=DIRECTION('center_axis',(0.,0.,-1.));
#4017=DIRECTION('ref_axis',(-1.,0.,0.));
#4018=DIRECTION('center_axis',(0.,0.,-1.));
#4019=DIRECTION('ref_axis',(-1.,0.,0.));
#4020=DIRECTION('center_axis',(0.,0.,-1.));
#4021=DIRECTION('ref_axis',(-1.,0.,0.));
#4022=DIRECTION('center_axis',(0.,0.,1.));
#4023=DIRECTION('ref_axis',(1.,0.,0.));
#4024=DIRECTION('center_axis',(0.,0.,-1.));
#4025=DIRECTION('ref_axis',(-1.,0.,0.));
#4026=DIRECTION('center_axis',(0.,0.,-1.));
#4027=DIRECTION('ref_axis',(-1.,0.,0.));
#4028=DIRECTION('center_axis',(0.,0.,1.));
#4029=DIRECTION('ref_axis',(-1.,0.,0.));
#4030=DIRECTION('center_axis',(0.,0.,1.));
#4031=DIRECTION('ref_axis',(-1.,-3.5527136788005E-15,0.));
#4032=DIRECTION('center_axis',(0.,0.,1.));
#4033=DIRECTION('ref_axis',(-1.,0.,0.));
#4034=DIRECTION('center_axis',(0.,0.,1.));
#4035=DIRECTION('ref_axis',(1.,0.,0.));
#4036=DIRECTION('center_axis',(0.,0.,1.));
#4037=DIRECTION('ref_axis',(-1.,1.77635683940025E-15,0.));
#4038=DIRECTION('center_axis',(0.,0.,1.));
#4039=DIRECTION('ref_axis',(-1.,0.,0.));
#4040=DIRECTION('center_axis',(0.,0.,1.));
#4041=DIRECTION('ref_axis',(1.,0.,0.));
#4042=DIRECTION('center_axis',(0.,0.,1.));
#4043=DIRECTION('ref_axis',(1.,0.,0.));
#4044=DIRECTION('center_axis',(0.,0.,1.));
#4045=DIRECTION('ref_axis',(1.,0.,0.));
#4046=DIRECTION('center_axis',(0.,0.,1.));
#4047=DIRECTION('ref_axis',(1.,0.,0.));
#4048=DIRECTION('center_axis',(0.,0.,1.));
#4049=DIRECTION('ref_axis',(1.,0.,0.));
#4050=DIRECTION('center_axis',(0.,0.,1.));
#4051=DIRECTION('ref_axis',(1.,0.,0.));
#4052=DIRECTION('center_axis',(0.,0.,-1.));
#4053=DIRECTION('ref_axis',(-1.,0.,0.));
#4054=DIRECTION('center_axis',(0.,0.,-1.));
#4055=DIRECTION('ref_axis',(-1.,0.,0.));
#4056=DIRECTION('center_axis',(0.,0.,-1.));
#4057=DIRECTION('ref_axis',(-1.,0.,0.));
#4058=DIRECTION('center_axis',(0.,0.,-1.));
#4059=DIRECTION('ref_axis',(-1.,0.,0.));
#4060=DIRECTION('center_axis',(0.,0.,-1.));
#4061=DIRECTION('ref_axis',(-1.,0.,0.));
#4062=DIRECTION('center_axis',(0.,0.,-1.));
#4063=DIRECTION('ref_axis',(-1.,0.,0.));
#4064=DIRECTION('axis',(0.,0.,1.));
#4065=DIRECTION('refdir',(1.,0.,0.));
#4066=DIRECTION('center_axis',(0.,0.,1.));
#4067=DIRECTION('ref_axis',(1.,0.,0.));
#4068=DIRECTION('center_axis',(0.,0.,1.));
#4069=DIRECTION('ref_axis',(1.,0.,0.));
#4070=DIRECTION('',(0.,0.,1.));
#4071=DIRECTION('center_axis',(0.,0.,1.));
#4072=DIRECTION('ref_axis',(1.,0.,0.));
#4073=DIRECTION('center_axis',(0.,0.,1.));
#4074=DIRECTION('ref_axis',(1.,0.,0.));
#4075=DIRECTION('center_axis',(0.,0.,1.));
#4076=DIRECTION('ref_axis',(1.,0.,0.));
#4077=DIRECTION('',(0.,0.,1.));
#4078=DIRECTION('center_axis',(0.,0.,1.));
#4079=DIRECTION('ref_axis',(1.,0.,0.));
#4080=DIRECTION('center_axis',(0.,0.,1.));
#4081=DIRECTION('ref_axis',(1.,0.,0.));
#4082=DIRECTION('center_axis',(0.,0.,1.));
#4083=DIRECTION('ref_axis',(1.,0.,0.));
#4084=DIRECTION('',(0.,0.,1.));
#4085=DIRECTION('center_axis',(0.,0.,1.));
#4086=DIRECTION('ref_axis',(1.,0.,0.));
#4087=DIRECTION('center_axis',(0.,0.,1.));
#4088=DIRECTION('ref_axis',(1.,0.,0.));
#4089=DIRECTION('center_axis',(0.,0.,1.));
#4090=DIRECTION('ref_axis',(1.,0.,0.));
#4091=DIRECTION('',(0.,0.,1.));
#4092=DIRECTION('center_axis',(0.,0.,1.));
#4093=DIRECTION('ref_axis',(1.,0.,0.));
#4094=DIRECTION('center_axis',(1.,0.,-6.93889390390723E-17));
#4095=DIRECTION('ref_axis',(-6.93889390390723E-17,0.,-1.));
#4096=DIRECTION('center_axis',(-1.,0.,6.93889390390723E-17));
#4097=DIRECTION('ref_axis',(6.93889390390723E-17,0.,1.));
#4098=DIRECTION('',(1.,0.,-6.93889390390723E-17));
#4099=DIRECTION('center_axis',(1.,0.,-6.93889390390723E-17));
#4100=DIRECTION('ref_axis',(-6.93889390390723E-17,0.,-1.));
#4101=DIRECTION('center_axis',(1.,0.,-6.93889390390723E-17));
#4102=DIRECTION('ref_axis',(-6.93889390390723E-17,0.,-1.));
#4103=DIRECTION('center_axis',(-1.,0.,6.93889390390723E-17));
#4104=DIRECTION('ref_axis',(6.93889390390723E-17,0.,1.));
#4105=DIRECTION('',(1.,0.,-6.93889390390723E-17));
#4106=DIRECTION('center_axis',(1.,0.,-6.93889390390723E-17));
#4107=DIRECTION('ref_axis',(6.93889390390723E-17,0.,1.));
#4108=DIRECTION('center_axis',(1.,0.,-6.93889390390723E-17));
#4109=DIRECTION('ref_axis',(-6.93889390390723E-17,0.,-1.));
#4110=DIRECTION('center_axis',(1.,0.,-6.93889390390723E-17));
#4111=DIRECTION('ref_axis',(-6.93889390390723E-17,0.,-1.));
#4112=DIRECTION('',(1.,0.,-6.93889390390723E-17));
#4113=DIRECTION('center_axis',(-1.,0.,-6.93889390390723E-17));
#4114=DIRECTION('ref_axis',(-6.93889390390723E-17,0.,1.));
#4115=DIRECTION('center_axis',(1.,0.,-6.93889390390723E-17));
#4116=DIRECTION('ref_axis',(-6.93889390390723E-17,0.,-1.));
#4117=DIRECTION('center_axis',(1.,0.,-6.93889390390723E-17));
#4118=DIRECTION('ref_axis',(6.93889390390723E-17,0.,1.));
#4119=DIRECTION('',(1.,0.,-6.93889390390723E-17));
#4120=DIRECTION('center_axis',(-1.,0.,-6.93889390390723E-17));
#4121=DIRECTION('ref_axis',(-6.93889390390723E-17,0.,1.));
#4122=DIRECTION('center_axis',(0.,1.,0.));
#4123=DIRECTION('ref_axis',(0.,0.,1.));
#4124=DIRECTION('',(-6.93889390390723E-17,0.,-1.));
#4125=DIRECTION('',(-1.,0.,0.));
#4126=DIRECTION('',(6.93889390390723E-17,0.,-1.));
#4127=DIRECTION('',(-1.,0.,0.));
#4128=DIRECTION('',(-1.,0.,0.));
#4129=DIRECTION('',(-6.93889390390723E-17,0.,-1.));
#4130=DIRECTION('',(-1.,0.,0.));
#4131=DIRECTION('',(6.93889390390723E-17,0.,-1.));
#4132=DIRECTION('center_axis',(0.,1.,0.));
#4133=DIRECTION('ref_axis',(0.,0.,1.));
#4134=DIRECTION('',(-6.93889390390723E-17,0.,-1.));
#4135=DIRECTION('',(-1.,0.,0.));
#4136=DIRECTION('',(6.93889390390723E-17,0.,-1.));
#4137=DIRECTION('',(-1.,0.,0.));
#4138=DIRECTION('',(-6.93889390390723E-17,0.,-1.));
#4139=DIRECTION('',(-1.,0.,0.));
#4140=DIRECTION('',(6.93889390390723E-17,0.,-1.));
#4141=DIRECTION('',(-1.,0.,0.));
#4142=DIRECTION('center_axis',(-1.,0.,6.93889390390723E-17));
#4143=DIRECTION('ref_axis',(6.93889390390723E-17,0.,1.));
#4144=DIRECTION('',(0.,-1.,0.));
#4145=DIRECTION('',(0.,-1.,0.));
#4146=DIRECTION('center_axis',(0.,0.,1.));
#4147=DIRECTION('ref_axis',(1.,0.,0.));
#4148=DIRECTION('',(0.,-1.,0.));
#4149=DIRECTION('center_axis',(-1.,0.,-6.93889390390723E-17));
#4150=DIRECTION('ref_axis',(-6.93889390390723E-17,0.,1.));
#4151=DIRECTION('',(0.,-1.,0.));
#4152=DIRECTION('center_axis',(0.,0.,1.));
#4153=DIRECTION('ref_axis',(1.,0.,0.));
#4154=DIRECTION('center_axis',(-1.,0.,6.93889390390723E-17));
#4155=DIRECTION('ref_axis',(6.93889390390723E-17,0.,1.));
#4156=DIRECTION('',(0.,-1.,0.));
#4157=DIRECTION('',(0.,-1.,0.));
#4158=DIRECTION('center_axis',(0.,0.,1.));
#4159=DIRECTION('ref_axis',(1.,0.,0.));
#4160=DIRECTION('',(0.,-1.,0.));
#4161=DIRECTION('center_axis',(-1.,0.,-6.93889390390723E-17));
#4162=DIRECTION('ref_axis',(-6.93889390390723E-17,0.,1.));
#4163=DIRECTION('',(0.,-1.,0.));
#4164=DIRECTION('center_axis',(0.,0.,1.));
#4165=DIRECTION('ref_axis',(1.,0.,0.));
#4166=DIRECTION('axis',(0.,0.,1.));
#4167=DIRECTION('refdir',(1.,0.,0.));
#4168=DIRECTION('center_axis',(0.,-1.,0.));
#4169=DIRECTION('ref_axis',(0.,0.,-1.));
#4170=DIRECTION('center_axis',(0.,-1.,0.));
#4171=DIRECTION('ref_axis',(0.,0.,-1.));
#4172=DIRECTION('center_axis',(0.,-1.,0.));
#4173=DIRECTION('ref_axis',(0.,0.,-1.));
#4174=DIRECTION('',(8.6595605623549E-17,0.70710678118655,-0.707106781186544));
#4175=DIRECTION('center_axis',(0.,1.,0.));
#4176=DIRECTION('ref_axis',(0.,0.,-1.));
#4177=DIRECTION('center_axis',(0.,-1.,0.));
#4178=DIRECTION('ref_axis',(0.,0.,-1.));
#4179=DIRECTION('center_axis',(0.,-1.,0.));
#4180=DIRECTION('ref_axis',(0.,0.,-1.));
#4181=DIRECTION('center_axis',(0.,-1.,0.));
#4182=DIRECTION('ref_axis',(0.,0.,-1.));
#4183=DIRECTION('',(8.65956056235496E-17,0.707106781186546,-0.707106781186549));
#4184=DIRECTION('center_axis',(0.,1.,0.));
#4185=DIRECTION('ref_axis',(0.,0.,-1.));
#4186=DIRECTION('center_axis',(0.,1.,0.));
#4187=DIRECTION('ref_axis',(0.,0.,1.));
#4188=DIRECTION('center_axis',(0.,1.,0.));
#4189=DIRECTION('ref_axis',(0.,0.,-1.));
#4190=DIRECTION('',(8.65956056235495E-17,-0.707106781186546,0.707106781186549));
#4191=DIRECTION('center_axis',(0.,-1.,0.));
#4192=DIRECTION('ref_axis',(0.,0.,-1.));
#4193=DIRECTION('center_axis',(0.,1.,0.));
#4194=DIRECTION('ref_axis',(0.,0.,1.));
#4195=DIRECTION('center_axis',(0.,1.,0.));
#4196=DIRECTION('ref_axis',(0.,0.,-1.));
#4197=DIRECTION('',(8.6595605623549E-17,-0.70710678118655,0.707106781186544));
#4198=DIRECTION('center_axis',(0.,-1.,0.));
#4199=DIRECTION('ref_axis',(0.,0.,-1.));
#4200=DIRECTION('center_axis',(0.,1.,0.));
#4201=DIRECTION('ref_axis',(0.,0.,1.));
#4202=DIRECTION('',(0.,-1.,0.));
#4203=DIRECTION('center_axis',(0.,1.,0.));
#4204=DIRECTION('ref_axis',(0.,0.,1.));
#4205=DIRECTION('center_axis',(0.,1.,0.));
#4206=DIRECTION('ref_axis',(0.,0.,1.));
#4207=DIRECTION('',(0.,-1.,0.));
#4208=DIRECTION('center_axis',(0.,1.,0.));
#4209=DIRECTION('ref_axis',(0.,0.,1.));
#4210=DIRECTION('',(0.,-1.,0.));
#4211=DIRECTION('center_axis',(0.,1.,0.));
#4212=DIRECTION('ref_axis',(0.,0.,1.));
#4213=DIRECTION('center_axis',(0.,-1.,0.));
#4214=DIRECTION('ref_axis',(0.,0.,-1.));
#4215=DIRECTION('center_axis',(0.,-1.,0.));
#4216=DIRECTION('ref_axis',(0.,0.,-1.));
#4217=DIRECTION('center_axis',(0.,-1.,0.));
#4218=DIRECTION('ref_axis',(0.,0.,-1.));
#4219=DIRECTION('center_axis',(0.,-1.,0.));
#4220=DIRECTION('ref_axis',(0.,0.,-1.));
#4221=DIRECTION('axis',(0.,0.,1.));
#4222=DIRECTION('refdir',(1.,0.,0.));
#4223=DIRECTION('center_axis',(-1.,0.,0.));
#4224=DIRECTION('ref_axis',(0.,0.,1.));
#4225=DIRECTION('',(-0.500000000000004,-1.0605752387249E-16,-0.866025403784436));
#4226=DIRECTION('center_axis',(-1.,0.,0.));
#4227=DIRECTION('ref_axis',(0.,0.,1.));
#4228=DIRECTION('center_axis',(-1.,0.,0.));
#4229=DIRECTION('ref_axis',(0.,0.,1.));
#4230=DIRECTION('center_axis',(-1.,0.,0.));
#4231=DIRECTION('ref_axis',(0.,0.,1.));
#4232=DIRECTION('center_axis',(-1.,0.,0.));
#4233=DIRECTION('ref_axis',(0.,0.,1.));
#4234=DIRECTION('center_axis',(-1.,0.,0.));
#4235=DIRECTION('ref_axis',(0.,0.,1.));
#4236=DIRECTION('center_axis',(-1.,0.,0.));
#4237=DIRECTION('ref_axis',(0.,0.,1.));
#4238=DIRECTION('center_axis',(1.,0.,0.));
#4239=DIRECTION('ref_axis',(0.,0.,-1.));
#4240=DIRECTION('center_axis',(1.,0.,0.));
#4241=DIRECTION('ref_axis',(0.,0.,-1.));
#4242=DIRECTION('center_axis',(1.,0.,0.));
#4243=DIRECTION('ref_axis',(0.,0.,-1.));
#4244=DIRECTION('center_axis',(0.,1.,1.22464679914735E-16));
#4245=DIRECTION('ref_axis',(0.,-1.22464679914735E-16,1.));
#4246=DIRECTION('center_axis',(-1.,0.,0.));
#4247=DIRECTION('ref_axis',(0.,0.,-1.));
#4248=DIRECTION('center_axis',(1.,0.,0.));
#4249=DIRECTION('ref_axis',(0.,0.,-1.));
#4250=DIRECTION('center_axis',(-1.,0.,0.));
#4251=DIRECTION('ref_axis',(0.,0.,1.));
#4252=DIRECTION('',(-0.707106781186548,8.65956056235493E-17,-0.707106781186548));
#4253=DIRECTION('center_axis',(-1.,0.,0.));
#4254=DIRECTION('ref_axis',(0.,0.,1.));
#4255=DIRECTION('center_axis',(-1.,0.,0.));
#4256=DIRECTION('ref_axis',(0.,0.,1.));
#4257=DIRECTION('center_axis',(-1.,0.,0.));
#4258=DIRECTION('ref_axis',(0.,0.,1.));
#4259=DIRECTION('',(1.,0.,0.));
#4260=DIRECTION('center_axis',(-1.,0.,0.));
#4261=DIRECTION('ref_axis',(0.,0.,1.));
#4262=DIRECTION('center_axis',(-1.,0.,0.));
#4263=DIRECTION('ref_axis',(0.,0.,1.));
#4264=DIRECTION('',(1.,0.,0.));
#4265=DIRECTION('center_axis',(-1.,0.,0.));
#4266=DIRECTION('ref_axis',(0.,0.,1.));
#4267=DIRECTION('center_axis',(-1.,0.,0.));
#4268=DIRECTION('ref_axis',(0.,0.,1.));
#4269=DIRECTION('',(0.707106781186468,8.6595605623559E-17,0.707106781186627));
#4270=DIRECTION('center_axis',(-1.,0.,0.));
#4271=DIRECTION('ref_axis',(0.,0.,1.));
#4272=DIRECTION('center_axis',(-1.,0.,0.));
#4273=DIRECTION('ref_axis',(0.,0.,1.));
#4274=DIRECTION('',(0.,-0.499999999999999,0.866025403784439));
#4275=DIRECTION('',(0.,1.,-1.11076864971324E-15));
#4276=DIRECTION('',(0.,-0.500000000000001,-0.866025403784438));
#4277=DIRECTION('',(0.,0.499999999999999,-0.866025403784439));
#4278=DIRECTION('',(0.,-1.,7.40512433142161E-16));
#4279=DIRECTION('',(0.,-0.500000000000001,-0.866025403784438));
#4280=DIRECTION('center_axis',(1.,0.,0.));
#4281=DIRECTION('ref_axis',(0.,0.,-1.));
#4282=DIRECTION('center_axis',(1.,0.,0.));
#4283=DIRECTION('ref_axis',(0.,0.,-1.));
#4284=DIRECTION('center_axis',(0.,-0.866025403784439,-0.499999999999999));
#4285=DIRECTION('ref_axis',(0.,0.499999999999999,-0.866025403784439));
#4286=DIRECTION('',(-1.,0.,0.));
#4287=DIRECTION('',(0.,-0.499999999999999,0.866025403784439));
#4288=DIRECTION('',(0.,-0.499999999999999,0.866025403784439));
#4289=DIRECTION('',(-1.,0.,0.));
#4290=DIRECTION('center_axis',(0.,1.11076864971324E-15,1.));
#4291=DIRECTION('ref_axis',(0.,-1.,1.11076864971324E-15));
#4292=DIRECTION('',(0.,1.,-1.11076864971324E-15));
#4293=DIRECTION('',(0.,1.,-1.11076864971324E-15));
#4294=DIRECTION('',(-1.,0.,0.));
#4295=DIRECTION('center_axis',(0.,0.866025403784438,-0.500000000000001));
#4296=DIRECTION('ref_axis',(0.,0.500000000000001,0.866025403784438));
#4297=DIRECTION('',(0.,-0.500000000000001,-0.866025403784438));
#4298=DIRECTION('',(0.,-0.500000000000001,-0.866025403784438));
#4299=DIRECTION('',(-1.,0.,0.));
#4300=DIRECTION('center_axis',(0.,0.866025403784439,0.499999999999999));
#4301=DIRECTION('ref_axis',(0.,-0.499999999999999,0.866025403784439));
#4302=DIRECTION('',(0.,0.499999999999999,-0.866025403784439));
#4303=DIRECTION('',(0.,0.499999999999999,-0.866025403784439));
#4304=DIRECTION('',(-1.,0.,0.));
#4305=DIRECTION('center_axis',(0.,-7.40512433142161E-16,-1.));
#4306=DIRECTION('ref_axis',(0.,1.,-7.40512433142161E-16));
#4307=DIRECTION('',(0.,-1.,7.40512433142161E-16));
#4308=DIRECTION('',(0.,-1.,7.40512433142161E-16));
#4309=DIRECTION('',(-1.,0.,0.));
#4310=DIRECTION('center_axis',(0.,0.866025403784438,-0.500000000000001));
#4311=DIRECTION('ref_axis',(0.,0.500000000000001,0.866025403784438));
#4312=DIRECTION('',(0.,-0.500000000000001,-0.866025403784438));
#4313=DIRECTION('',(0.,-0.500000000000001,-0.866025403784438));
#4314=DIRECTION('center_axis',(1.,0.,0.));
#4315=DIRECTION('ref_axis',(0.,0.,-1.));
#4316=DIRECTION('center_axis',(1.,0.,0.));
#4317=DIRECTION('ref_axis',(0.,0.,-1.));
#4318=DIRECTION('center_axis',(1.,0.,0.));
#4319=DIRECTION('ref_axis',(0.,0.,-1.));
#4320=DIRECTION('center_axis',(1.,0.,0.));
#4321=DIRECTION('ref_axis',(0.,0.,-1.));
#4322=DIRECTION('center_axis',(1.,0.,0.));
#4323=DIRECTION('ref_axis',(0.,0.,-1.));
#4324=DIRECTION('center_axis',(1.,0.,0.));
#4325=DIRECTION('ref_axis',(0.,0.,-1.));
#4326=DIRECTION('axis',(0.,0.,1.));
#4327=DIRECTION('refdir',(1.,0.,0.));
#4328=DIRECTION('center_axis',(-1.,0.,0.));
#4329=DIRECTION('ref_axis',(0.,0.,1.));
#4330=DIRECTION('center_axis',(-1.,0.,0.));
#4331=DIRECTION('ref_axis',(0.,0.,1.));
#4332=DIRECTION('',(1.,0.,0.));
#4333=DIRECTION('center_axis',(-1.,0.,0.));
#4334=DIRECTION('ref_axis',(0.,0.,1.));
#4335=DIRECTION('center_axis',(-1.,0.,0.));
#4336=DIRECTION('ref_axis',(0.,0.,1.));
#4337=DIRECTION('center_axis',(-1.,0.,0.));
#4338=DIRECTION('ref_axis',(0.,0.,1.));
#4339=DIRECTION('',(-1.,0.,0.));
#4340=DIRECTION('center_axis',(-1.,0.,0.));
#4341=DIRECTION('ref_axis',(0.,0.,1.));
#4342=DIRECTION('center_axis',(-1.,0.,0.));
#4343=DIRECTION('ref_axis',(0.,0.,1.));
#4344=DIRECTION('center_axis',(1.,0.,0.));
#4345=DIRECTION('ref_axis',(0.,0.,-1.));
#4346=DIRECTION('axis',(0.,0.,1.));
#4347=DIRECTION('refdir',(1.,0.,0.));
#4348=DIRECTION('center_axis',(-1.,0.,0.));
#4349=DIRECTION('ref_axis',(0.,0.,1.));
#4350=DIRECTION('',(-0.500000000000005,-1.0605752387249E-16,-0.866025403784436));
#4351=DIRECTION('center_axis',(-1.,0.,0.));
#4352=DIRECTION('ref_axis',(0.,0.,1.));
#4353=DIRECTION('center_axis',(-1.,0.,0.));
#4354=DIRECTION('ref_axis',(0.,0.,1.));
#4355=DIRECTION('center_axis',(-1.,0.,0.));
#4356=DIRECTION('ref_axis',(0.,0.,1.));
#4357=DIRECTION('center_axis',(-1.,0.,0.));
#4358=DIRECTION('ref_axis',(0.,0.,1.));
#4359=DIRECTION('center_axis',(-1.,0.,0.));
#4360=DIRECTION('ref_axis',(0.,0.,1.));
#4361=DIRECTION('center_axis',(-1.,0.,0.));
#4362=DIRECTION('ref_axis',(0.,0.,1.));
#4363=DIRECTION('center_axis',(1.,0.,0.));
#4364=DIRECTION('ref_axis',(0.,0.,-1.));
#4365=DIRECTION('center_axis',(1.,0.,0.));
#4366=DIRECTION('ref_axis',(0.,0.,-1.));
#4367=DIRECTION('center_axis',(1.,0.,0.));
#4368=DIRECTION('ref_axis',(0.,0.,-1.));
#4369=DIRECTION('center_axis',(0.,1.,1.22464679914735E-16));
#4370=DIRECTION('ref_axis',(0.,-1.22464679914735E-16,1.));
#4371=DIRECTION('center_axis',(-1.,0.,0.));
#4372=DIRECTION('ref_axis',(0.,0.,-1.));
#4373=DIRECTION('center_axis',(-1.,0.,0.));
#4374=DIRECTION('ref_axis',(0.,0.,1.));
#4375=DIRECTION('center_axis',(-1.,0.,0.));
#4376=DIRECTION('ref_axis',(0.,0.,1.));
#4377=DIRECTION('',(0.707106781186465,8.65956056235594E-17,0.70710678118663));
#4378=DIRECTION('center_axis',(-1.,0.,0.));
#4379=DIRECTION('ref_axis',(0.,0.,1.));
#4380=DIRECTION('center_axis',(-1.,0.,0.));
#4381=DIRECTION('ref_axis',(0.,0.,1.));
#4382=DIRECTION('',(1.,0.,0.));
#4383=DIRECTION('center_axis',(-1.,0.,0.));
#4384=DIRECTION('ref_axis',(0.,0.,1.));
#4385=DIRECTION('center_axis',(-1.,0.,0.));
#4386=DIRECTION('ref_axis',(0.,0.,1.));
#4387=DIRECTION('center_axis',(-1.,0.,0.));
#4388=DIRECTION('ref_axis',(0.,0.,1.));
#4389=DIRECTION('',(1.,0.,0.));
#4390=DIRECTION('center_axis',(-1.,0.,0.));
#4391=DIRECTION('ref_axis',(0.,0.,1.));
#4392=DIRECTION('center_axis',(1.,0.,0.));
#4393=DIRECTION('ref_axis',(0.,0.,-1.));
#4394=DIRECTION('',(-0.707106781186548,8.65956056235492E-17,-0.707106781186547));
#4395=DIRECTION('center_axis',(-1.,0.,0.));
#4396=DIRECTION('ref_axis',(0.,0.,1.));
#4397=DIRECTION('center_axis',(-1.,0.,0.));
#4398=DIRECTION('ref_axis',(0.,0.,1.));
#4399=DIRECTION('',(0.,-0.499999999999998,0.866025403784439));
#4400=DIRECTION('',(0.,1.,-8.62690909857269E-16));
#4401=DIRECTION('',(0.,-0.500000000000001,-0.866025403784438));
#4402=DIRECTION('',(0.,0.499999999999999,-0.866025403784439));
#4403=DIRECTION('',(0.,-1.,1.47889870261246E-15));
#4404=DIRECTION('',(0.,-0.500000000000001,-0.866025403784438));
#4405=DIRECTION('center_axis',(1.,0.,0.));
#4406=DIRECTION('ref_axis',(0.,0.,-1.));
#4407=DIRECTION('center_axis',(1.,0.,0.));
#4408=DIRECTION('ref_axis',(0.,0.,-1.));
#4409=DIRECTION('center_axis',(0.,-0.86602540378444,-0.499999999999998));
#4410=DIRECTION('ref_axis',(0.,0.499999999999998,-0.86602540378444));
#4411=DIRECTION('',(-1.,0.,0.));
#4412=DIRECTION('',(0.,-0.499999999999998,0.866025403784439));
#4413=DIRECTION('',(0.,-0.499999999999998,0.866025403784439));
#4414=DIRECTION('',(-1.,0.,0.));
#4415=DIRECTION('center_axis',(0.,8.62690909857269E-16,1.));
#4416=DIRECTION('ref_axis',(0.,-1.,8.62690909857269E-16));
#4417=DIRECTION('',(0.,1.,-8.62690909857269E-16));
#4418=DIRECTION('',(0.,1.,-8.62690909857269E-16));
#4419=DIRECTION('',(-1.,0.,0.));
#4420=DIRECTION('center_axis',(0.,0.866025403784438,-0.500000000000001));
#4421=DIRECTION('ref_axis',(0.,0.500000000000001,0.866025403784438));
#4422=DIRECTION('',(0.,-0.500000000000001,-0.866025403784438));
#4423=DIRECTION('',(0.,-0.500000000000001,-0.866025403784438));
#4424=DIRECTION('',(-1.,0.,0.));
#4425=DIRECTION('center_axis',(0.,0.866025403784439,0.499999999999999));
#4426=DIRECTION('ref_axis',(0.,-0.499999999999999,0.866025403784439));
#4427=DIRECTION('',(0.,0.499999999999999,-0.866025403784439));
#4428=DIRECTION('',(0.,0.499999999999999,-0.866025403784439));
#4429=DIRECTION('',(-1.,0.,0.));
#4430=DIRECTION('center_axis',(0.,-1.47889870261246E-15,-1.));
#4431=DIRECTION('ref_axis',(0.,1.,-1.47889870261246E-15));
#4432=DIRECTION('',(0.,-1.,1.47889870261246E-15));
#4433=DIRECTION('',(0.,-1.,1.47889870261246E-15));
#4434=DIRECTION('',(-1.,0.,0.));
#4435=DIRECTION('center_axis',(0.,0.866025403784438,-0.500000000000001));
#4436=DIRECTION('ref_axis',(0.,0.500000000000001,0.866025403784438));
#4437=DIRECTION('',(0.,-0.500000000000001,-0.866025403784438));
#4438=DIRECTION('',(0.,-0.500000000000001,-0.866025403784438));
#4439=DIRECTION('center_axis',(-1.,0.,0.));
#4440=DIRECTION('ref_axis',(0.,0.,1.));
#4441=DIRECTION('center_axis',(-1.,0.,0.));
#4442=DIRECTION('ref_axis',(0.,0.,1.));
#4443=DIRECTION('center_axis',(-1.,0.,0.));
#4444=DIRECTION('ref_axis',(0.,0.,1.));
#4445=DIRECTION('center_axis',(-1.,0.,0.));
#4446=DIRECTION('ref_axis',(0.,0.,1.));
#4447=DIRECTION('center_axis',(-1.,0.,0.));
#4448=DIRECTION('ref_axis',(0.,0.,1.));
#4449=DIRECTION('center_axis',(-1.,0.,0.));
#4450=DIRECTION('ref_axis',(0.,0.,1.));
#4451=DIRECTION('',(0.,0.,1.));
#4452=DIRECTION('',(1.,0.,0.));
#4453=DIRECTION('',(-8.24019699893244E-18,-0.270250608069463,-0.962790012847083));
#4454=DIRECTION('',(-2.26682217091051E-17,0.962790012847083,-0.270250608069463));
#4455=DIRECTION('',(0.,0.,1.));
#4456=DIRECTION('',(1.,0.,0.));
#4457=DIRECTION('',(1.05847197524526E-16,-8.73654476623684E-16,1.));
#4458=DIRECTION('',(1.66533453693773E-16,1.,8.73654476623684E-16));
#4459=DIRECTION('',(4.57297847870545E-16,-6.68346614730151E-17,1.));
#4460=DIRECTION('',(2.22044604925031E-16,1.,6.6834661473015E-17));
#4461=DIRECTION('',(0.,0.,1.));
#4462=DIRECTION('',(1.,0.,0.));
#4463=DIRECTION('',(1.,8.73654476623684E-16,-1.05847197524525E-16));
#4464=DIRECTION('',(-1.05847197524526E-16,8.73654476623684E-16,-1.));
#4465=DIRECTION('',(-1.,0.,0.));
#4466=DIRECTION('',(0.,0.,1.));
#4467=DIRECTION('',(0.,0.,-1.));
#4468=DIRECTION('',(0.923728021347068,0.383049008063238,0.));
#4469=DIRECTION('',(0.,0.,-1.));
#4470=DIRECTION('',(0.923728021347068,0.383049008063238,0.));
#4471=DIRECTION('',(0.970061834989277,0.242858057921158,1.09495702827839E-16));
#4472=DIRECTION('',(-1.05847197524526E-16,8.73654476623686E-16,-1.));
#4473=DIRECTION('',(0.,0.,1.));
#4474=DIRECTION('',(1.,0.,0.));
#4475=DIRECTION('',(1.69223923597971E-17,-0.154710762113361,0.987959806918431));
#4476=DIRECTION('',(1.71866738736269E-17,-0.987959806918431,-0.154710762113361));
#4477=DIRECTION('',(1.,8.73654476623684E-16,-1.05847197524525E-16));
#4478=DIRECTION('',(-1.05847197524526E-16,8.73654476623684E-16,-1.));
#4479=DIRECTION('',(-1.,0.,0.));
#4480=DIRECTION('',(0.,0.,1.));
#4481=DIRECTION('',(1.,8.73654476623685E-16,-1.05847197524525E-16));
#4482=DIRECTION('',(-1.05847197524526E-16,8.73654476623685E-16,-1.));
#4483=DIRECTION('',(0.999985539774282,0.00537775439552218,-1.01147367748328E-16));
#4484=DIRECTION('',(-1.05847197524526E-16,8.73654476623685E-16,-1.));
#4485=DIRECTION('',(1.,8.73654476623685E-16,-1.05847197524525E-16));
#4486=DIRECTION('',(-1.05847197524526E-16,8.73654476623685E-16,-1.));
#4487=CARTESIAN_POINT('',(0.,0.,0.));
#4488=CARTESIAN_POINT('',(0.,0.,0.));
#4489=CARTESIAN_POINT('Origin',(275.,-425.,0.));
#4490=CARTESIAN_POINT('',(275.,-425.,80.));
#4491=CARTESIAN_POINT('',(275.,-425.,-80.));
#4492=CARTESIAN_POINT('Origin',(275.,-425.,0.));
#4493=CARTESIAN_POINT('',(275.,425.,-79.9999999999998));
#4494=CARTESIAN_POINT('',(275.,-425.,-80.));
#4495=CARTESIAN_POINT('',(275.,425.,80.0000000000002));
#4496=CARTESIAN_POINT('Origin',(275.,425.,1.56142466891288E-13));
#4497=CARTESIAN_POINT('',(275.,-425.,80.));
#4498=CARTESIAN_POINT('',(275.,-425.,-75.));
#4499=CARTESIAN_POINT('',(275.,425.,-74.9999999999998));
#4500=CARTESIAN_POINT('',(275.,-425.,-75.));
#4501=CARTESIAN_POINT('',(275.,-425.,75.));
#4502=CARTESIAN_POINT('Origin',(275.,-425.,0.));
#4503=CARTESIAN_POINT('',(275.,425.,75.0000000000002));
#4504=CARTESIAN_POINT('',(275.,-425.,75.));
#4505=CARTESIAN_POINT('Origin',(275.,425.,1.56142466891288E-13));
#4506=CARTESIAN_POINT('Origin',(-275.,-425.,0.));
#4507=CARTESIAN_POINT('',(-275.,-425.,80.));
#4508=CARTESIAN_POINT('',(-275.,-425.,-80.));
#4509=CARTESIAN_POINT('Origin',(-275.,-425.,0.));
#4510=CARTESIAN_POINT('',(-275.,425.,80.0000000000002));
#4511=CARTESIAN_POINT('',(-275.,-425.,80.));
#4512=CARTESIAN_POINT('',(-275.,425.,-79.9999999999998));
#4513=CARTESIAN_POINT('Origin',(-275.,425.,1.56142466891288E-13));
#4514=CARTESIAN_POINT('',(-275.,-425.,-80.));
#4515=CARTESIAN_POINT('',(-275.,-425.,75.));
#4516=CARTESIAN_POINT('',(-275.,-425.,-75.));
#4517=CARTESIAN_POINT('Origin',(-275.,-425.,0.));
#4518=CARTESIAN_POINT('',(-275.,425.,-74.9999999999998));
#4519=CARTESIAN_POINT('',(-275.,-425.,-75.));
#4520=CARTESIAN_POINT('',(-275.,425.,75.0000000000002));
#4521=CARTESIAN_POINT('Origin',(-275.,425.,1.56142466891288E-13));
#4522=CARTESIAN_POINT('',(-275.,-425.,75.));
#4523=CARTESIAN_POINT('Origin',(275.,-425.,0.));
#4524=CARTESIAN_POINT('',(275.,-425.,-80.));
#4525=CARTESIAN_POINT('',(275.,-425.,80.));
#4526=CARTESIAN_POINT('Origin',(275.,-425.,-80.));
#4527=CARTESIAN_POINT('',(275.,425.,-79.9999999999998));
#4528=CARTESIAN_POINT('Origin',(275.,425.,1.56142466891288E-13));
#4529=CARTESIAN_POINT('',(275.,425.,80.0000000000002));
#4530=CARTESIAN_POINT('Origin',(275.,-425.,80.));
#4531=CARTESIAN_POINT('Origin',(275.,-425.,0.));
#4532=CARTESIAN_POINT('',(275.,-425.,75.));
#4533=CARTESIAN_POINT('',(275.,-425.,-75.));
#4534=CARTESIAN_POINT('Origin',(275.,-425.,-75.));
#4535=CARTESIAN_POINT('',(275.,425.,-74.9999999999998));
#4536=CARTESIAN_POINT('Origin',(275.,425.,1.56142466891288E-13));
#4537=CARTESIAN_POINT('',(275.,425.,75.0000000000002));
#4538=CARTESIAN_POINT('Origin',(275.,-425.,75.));
#4539=CARTESIAN_POINT('',(0.,0.,0.));
#4540=CARTESIAN_POINT('Origin',(-82.5,120.,10.));
#4541=CARTESIAN_POINT('',(-78.5,120.,10.));
#4542=CARTESIAN_POINT('Origin',(-82.5,120.,10.));
#4543=CARTESIAN_POINT('',(-78.5,120.,0.));
#4544=CARTESIAN_POINT('',(-78.5,120.,10.));
#4545=CARTESIAN_POINT('Origin',(-82.5,120.,0.));
#4546=CARTESIAN_POINT('Origin',(-50.,87.5,10.));
#4547=CARTESIAN_POINT('',(-46.,87.5,10.));
#4548=CARTESIAN_POINT('Origin',(-50.,87.5,10.));
#4549=CARTESIAN_POINT('',(-46.,87.5,0.));
#4550=CARTESIAN_POINT('',(-46.,87.5,10.));
#4551=CARTESIAN_POINT('Origin',(-50.,87.5,0.));
#4552=CARTESIAN_POINT('Origin',(-17.5,120.,10.));
#4553=CARTESIAN_POINT('',(-13.5,120.,10.));
#4554=CARTESIAN_POINT('Origin',(-17.5,120.,10.));
#4555=CARTESIAN_POINT('',(-13.5,120.,0.));
#4556=CARTESIAN_POINT('',(-13.5,120.,10.));
#4557=CARTESIAN_POINT('Origin',(-17.5,120.,0.));
#4558=CARTESIAN_POINT('Origin',(-50.,152.5,10.));
#4559=CARTESIAN_POINT('',(-46.,152.5,10.));
#4560=CARTESIAN_POINT('Origin',(-50.,152.5,10.));
#4561=CARTESIAN_POINT('',(-46.,152.5,0.));
#4562=CARTESIAN_POINT('',(-46.,152.5,10.));
#4563=CARTESIAN_POINT('Origin',(-50.,152.5,0.));
#4564=CARTESIAN_POINT('Origin',(-20.,15.,10.));
#4565=CARTESIAN_POINT('',(-14.25,15.,10.));
#4566=CARTESIAN_POINT('Origin',(-20.,15.,10.));
#4567=CARTESIAN_POINT('',(-14.25,15.,0.));
#4568=CARTESIAN_POINT('',(-14.25,15.,10.));
#4569=CARTESIAN_POINT('Origin',(-20.,15.,0.));
#4570=CARTESIAN_POINT('Origin',(-80.,15.,10.));
#4571=CARTESIAN_POINT('',(-74.25,15.,10.));
#4572=CARTESIAN_POINT('Origin',(-80.,15.,10.));
#4573=CARTESIAN_POINT('',(-74.25,15.,0.));
#4574=CARTESIAN_POINT('',(-74.25,15.,10.));
#4575=CARTESIAN_POINT('Origin',(-80.,15.,0.));
#4576=CARTESIAN_POINT('Origin',(-50.,120.,10.));
#4577=CARTESIAN_POINT('',(-100.,0.,10.));
#4578=CARTESIAN_POINT('',(0.,0.,10.));
#4579=CARTESIAN_POINT('',(0.,0.,10.));
#4580=CARTESIAN_POINT('',(8.67361737988404E-14,120.,10.));
#4581=CARTESIAN_POINT('',(0.,0.,10.));
#4582=CARTESIAN_POINT('',(-100.,119.999999999999,10.));
#4583=CARTESIAN_POINT('Origin',(-50.,120.,10.));
#4584=CARTESIAN_POINT('',(-100.,0.,10.));
#4585=CARTESIAN_POINT('Origin',(-50.,120.,0.));
#4586=CARTESIAN_POINT('',(-100.,0.,0.));
#4587=CARTESIAN_POINT('',(0.,0.,0.));
#4588=CARTESIAN_POINT('',(0.,0.,0.));
#4589=CARTESIAN_POINT('',(-100.,119.999999999999,0.));
#4590=CARTESIAN_POINT('',(-100.,0.,0.));
#4591=CARTESIAN_POINT('',(8.67361737988404E-14,120.,0.));
#4592=CARTESIAN_POINT('Origin',(-50.,120.,0.));
#4593=CARTESIAN_POINT('',(0.,0.,0.));
#4594=CARTESIAN_POINT('Origin',(0.,0.,10.));
#4595=CARTESIAN_POINT('',(0.,0.,10.));
#4596=CARTESIAN_POINT('',(-100.,0.,10.));
#4597=CARTESIAN_POINT('Origin',(0.,0.,10.));
#4598=CARTESIAN_POINT('',(8.67361737988404E-14,120.,10.));
#4599=CARTESIAN_POINT('Origin',(-50.,120.,10.));
#4600=CARTESIAN_POINT('',(-100.,119.999999999999,10.));
#4601=CARTESIAN_POINT('Origin',(-100.,0.,10.));
#4602=CARTESIAN_POINT('',(0.,0.,0.));
#4603=CARTESIAN_POINT('Origin',(0.,-30.,370.));
#4604=CARTESIAN_POINT('',(8.57252759403147E-16,-30.,393.));
#4605=CARTESIAN_POINT('Origin',(0.,-30.,400.));
#4606=CARTESIAN_POINT('',(8.57252759403147E-16,-6.99999999999999,370.));
#4607=CARTESIAN_POINT('Origin',(8.57252759403147E-16,-30.,370.));
#4608=CARTESIAN_POINT('Origin',(0.,1.04083408558608E-14,370.));
#4609=CARTESIAN_POINT('Origin',(0.,-30.,370.));
#4610=CARTESIAN_POINT('',(1.22464679914735E-15,-10.,370.));
#4611=CARTESIAN_POINT('Origin',(0.,-3.46944695195361E-15,370.));
#4612=CARTESIAN_POINT('',(1.22464679914735E-15,-30.,390.));
#4613=CARTESIAN_POINT('Origin',(1.22464679914735E-15,-30.,370.));
#4614=CARTESIAN_POINT('Origin',(0.,-30.,400.));
#4615=CARTESIAN_POINT('Origin',(-50.,-185.,400.));
#4616=CARTESIAN_POINT('',(-8.35164654424502,-185.,405.5));
#4617=CARTESIAN_POINT('Ctrl Pts',(-8.35164654424504,-185.,394.5));
#4618=CARTESIAN_POINT('Ctrl Pts',(-8.35164654424504,-184.290235405321,394.5));
#4619=CARTESIAN_POINT('Ctrl Pts',(-8.45174305106268,-183.547853071563,394.64504316336));
#4620=CARTESIAN_POINT('Ctrl Pts',(-8.78438651561337,-182.199599169859,395.210212504666));
#4621=CARTESIAN_POINT('Ctrl Pts',(-9.00975031605896,-181.591824169425,395.630001237523));
#4622=CARTESIAN_POINT('Ctrl Pts',(-9.41491390301225,-180.632042150617,396.589783256331));
#4623=CARTESIAN_POINT('Ctrl Pts',(-9.62434109787453,-180.210790188028,397.198189638843));
#4624=CARTESIAN_POINT('Ctrl Pts',(-9.91836499005242,-179.644390383362,398.549441755203));
#4625=CARTESIAN_POINT('Ctrl Pts',(-10.,-179.5,399.293247535323));
#4626=CARTESIAN_POINT('Ctrl Pts',(-10.,-179.5,400.706752464677));
#4627=CARTESIAN_POINT('Ctrl Pts',(-9.91836499005242,-179.644390383362,401.450558244797));
#4628=CARTESIAN_POINT('Ctrl Pts',(-9.62434109787453,-180.210790188028,402.801810361157));
#4629=CARTESIAN_POINT('Ctrl Pts',(-9.41491390301225,-180.632042150617,403.410216743669));
#4630=CARTESIAN_POINT('Ctrl Pts',(-9.00975031605896,-181.591824169425,404.369998762477));
#4631=CARTESIAN_POINT('Ctrl Pts',(-8.78438651561337,-182.199599169859,404.789787495334));
#4632=CARTESIAN_POINT('Ctrl Pts',(-8.45174305106268,-183.547853071563,405.35495683664));
#4633=CARTESIAN_POINT('Ctrl Pts',(-8.35164654424506,-184.290235405321,405.5));
#4634=CARTESIAN_POINT('Ctrl Pts',(-8.35164654424506,-185.70976459468,405.5));
#4635=CARTESIAN_POINT('Ctrl Pts',(-8.45174305106268,-186.452146928437,405.35495683664));
#4636=CARTESIAN_POINT('Ctrl Pts',(-8.78438651561337,-187.800400830141,404.789787495334));
#4637=CARTESIAN_POINT('Ctrl Pts',(-9.00975031605896,-188.408175830575,404.369998762477));
#4638=CARTESIAN_POINT('Ctrl Pts',(-9.41491390301225,-189.367957849383,403.410216743669));
#4639=CARTESIAN_POINT('Ctrl Pts',(-9.62434109787455,-189.789209811972,402.801810361157));
#4640=CARTESIAN_POINT('Ctrl Pts',(-9.91836499005243,-190.355609616638,401.450558244797));
#4641=CARTESIAN_POINT('Ctrl Pts',(-10.,-190.5,400.706752464677));
#4642=CARTESIAN_POINT('Ctrl Pts',(-10.,-190.5,399.293247535323));
#4643=CARTESIAN_POINT('Ctrl Pts',(-9.9183649900524,-190.355609616638,398.549441755203));
#4644=CARTESIAN_POINT('Ctrl Pts',(-9.62434109787451,-189.789209811972,397.198189638843));
#4645=CARTESIAN_POINT('Ctrl Pts',(-9.41491390301225,-189.367957849383,396.589783256331));
#4646=CARTESIAN_POINT('Ctrl Pts',(-9.00975031605896,-188.408175830575,395.630001237523));
#4647=CARTESIAN_POINT('Ctrl Pts',(-8.78438651561337,-187.800400830141,395.210212504666));
#4648=CARTESIAN_POINT('Ctrl Pts',(-8.45174305106268,-186.452146928437,394.64504316336));
#4649=CARTESIAN_POINT('Ctrl Pts',(-8.35164654424504,-185.70976459468,394.5));
#4650=CARTESIAN_POINT('Ctrl Pts',(-8.35164654424504,-185.,394.5));
#4651=CARTESIAN_POINT('',(-4.33012701892219,-185.,405.5));
#4652=CARTESIAN_POINT('',(-50.,-185.,405.5));
#4653=CARTESIAN_POINT('',(-4.33012701892219,-185.,394.5));
#4654=CARTESIAN_POINT('Ctrl Pts',(-4.33012701892219,-185.,405.5));
#4655=CARTESIAN_POINT('Ctrl Pts',(-4.33012701892219,-185.37385187057,405.5));
#4656=CARTESIAN_POINT('Ctrl Pts',(-4.37998128622333,-185.746075739511,405.461618176925));
#4657=CARTESIAN_POINT('Ctrl Pts',(-4.55888740591996,-186.468280486434,405.313196276448));
#4658=CARTESIAN_POINT('Ctrl Pts',(-4.68703690659531,-186.81849775152,405.203220220576));
#4659=CARTESIAN_POINT('Ctrl Pts',(-5.13065352868785,-187.815687292683,404.779503215329));
#4660=CARTESIAN_POINT('Ctrl Pts',(-5.50080088534137,-188.411054784548,404.367119808505));
#4661=CARTESIAN_POINT('Ctrl Pts',(-6.13076939848926,-189.353835745446,403.424338847606));
#4662=CARTESIAN_POINT('Ctrl Pts',(-6.44230837852261,-189.773691234096,402.828149962177));
#4663=CARTESIAN_POINT('Ctrl Pts',(-6.87828608217357,-190.347486404219,401.48018651652));
#4664=CARTESIAN_POINT('Ctrl Pts',(-7.00000000000001,-190.5,400.726925774374));
#4665=CARTESIAN_POINT('Ctrl Pts',(-7.00000000000001,-190.5,399.273074225626));
#4666=CARTESIAN_POINT('Ctrl Pts',(-6.87828608217358,-190.347486404219,398.51981348348));
#4667=CARTESIAN_POINT('Ctrl Pts',(-6.44230837852261,-189.773691234096,397.171850037823));
#4668=CARTESIAN_POINT('Ctrl Pts',(-6.13076939848926,-189.353835745446,396.575661152394));
#4669=CARTESIAN_POINT('Ctrl Pts',(-5.50080088534137,-188.411054784548,395.632880191495));
#4670=CARTESIAN_POINT('Ctrl Pts',(-5.13065352868785,-187.815687292683,395.220496784671));
#4671=CARTESIAN_POINT('Ctrl Pts',(-4.68703690659531,-186.81849775152,394.796779779424));
#4672=CARTESIAN_POINT('Ctrl Pts',(-4.55888740591996,-186.468280486434,394.686803723552));
#4673=CARTESIAN_POINT('Ctrl Pts',(-4.37998128622333,-185.746075739511,394.538381823075));
#4674=CARTESIAN_POINT('Ctrl Pts',(-4.3301270189222,-185.37385187057,394.5));
#4675=CARTESIAN_POINT('Ctrl Pts',(-4.3301270189222,-185.,394.5));
#4676=CARTESIAN_POINT('Ctrl Pts',(-4.3301270189222,-185.,394.5));
#4677=CARTESIAN_POINT('Ctrl Pts',(-4.3301270189222,-184.626148129431,394.5));
#4678=CARTESIAN_POINT('Ctrl Pts',(-4.37998128622333,-184.25392426049,394.538381823075));
#4679=CARTESIAN_POINT('Ctrl Pts',(-4.55888740591996,-183.531719513566,394.686803723552));
#4680=CARTESIAN_POINT('Ctrl Pts',(-4.68703690659531,-183.18150224848,394.796779779424));
#4681=CARTESIAN_POINT('Ctrl Pts',(-5.13065352868785,-182.184312707317,395.220496784671));
#4682=CARTESIAN_POINT('Ctrl Pts',(-5.50080088534137,-181.588945215453,395.632880191495));
#4683=CARTESIAN_POINT('Ctrl Pts',(-6.13076939848926,-180.646164254554,396.575661152394));
#4684=CARTESIAN_POINT('Ctrl Pts',(-6.44230837852252,-180.226308765904,397.171850037822));
#4685=CARTESIAN_POINT('Ctrl Pts',(-6.87828608217351,-179.652513595781,398.51981348348));
#4686=CARTESIAN_POINT('Ctrl Pts',(-7.00000000000001,-179.5,399.273074225626));
#4687=CARTESIAN_POINT('Ctrl Pts',(-7.00000000000001,-179.5,400.726925774374));
#4688=CARTESIAN_POINT('Ctrl Pts',(-6.87828608217354,-179.652513595781,401.48018651652));
#4689=CARTESIAN_POINT('Ctrl Pts',(-6.44230837852263,-180.226308765904,402.828149962177));
#4690=CARTESIAN_POINT('Ctrl Pts',(-6.13076939848926,-180.646164254554,403.424338847606));
#4691=CARTESIAN_POINT('Ctrl Pts',(-5.50080088534137,-181.588945215453,404.367119808505));
#4692=CARTESIAN_POINT('Ctrl Pts',(-5.13065352868785,-182.184312707317,404.779503215329));
#4693=CARTESIAN_POINT('Ctrl Pts',(-4.68703690659531,-183.18150224848,405.203220220576));
#4694=CARTESIAN_POINT('Ctrl Pts',(-4.55888740591996,-183.531719513566,405.313196276448));
#4695=CARTESIAN_POINT('Ctrl Pts',(-4.37998128622333,-184.25392426049,405.461618176925));
#4696=CARTESIAN_POINT('Ctrl Pts',(-4.33012701892219,-184.626148129431,405.5));
#4697=CARTESIAN_POINT('Ctrl Pts',(-4.33012701892219,-185.,405.5));
#4698=CARTESIAN_POINT('Origin',(-50.,-185.,400.));
#4699=CARTESIAN_POINT('',(4.33012701892219,-185.,394.5));
#4700=CARTESIAN_POINT('',(4.3301270189222,-185.,405.5));
#4701=CARTESIAN_POINT('Ctrl Pts',(4.3301270189222,-185.,394.5));
#4702=CARTESIAN_POINT('Ctrl Pts',(4.3301270189222,-185.37385187057,394.5));
#4703=CARTESIAN_POINT('Ctrl Pts',(4.37998128622333,-185.746075739511,394.538381823075));
#4704=CARTESIAN_POINT('Ctrl Pts',(4.55888740591996,-186.468280486434,394.686803723552));
#4705=CARTESIAN_POINT('Ctrl Pts',(4.68703690659531,-186.81849775152,394.796779779424));
#4706=CARTESIAN_POINT('Ctrl Pts',(5.13065352868785,-187.815687292683,395.220496784671));
#4707=CARTESIAN_POINT('Ctrl Pts',(5.50080088534137,-188.411054784548,395.632880191495));
#4708=CARTESIAN_POINT('Ctrl Pts',(6.13076939848926,-189.353835745446,396.575661152394));
#4709=CARTESIAN_POINT('Ctrl Pts',(6.44230837852261,-189.773691234096,397.171850037823));
#4710=CARTESIAN_POINT('Ctrl Pts',(6.87828608217358,-190.347486404219,398.51981348348));
#4711=CARTESIAN_POINT('Ctrl Pts',(7.00000000000001,-190.5,399.273074225626));
#4712=CARTESIAN_POINT('Ctrl Pts',(7.00000000000001,-190.5,400.726925774374));
#4713=CARTESIAN_POINT('Ctrl Pts',(6.87828608217357,-190.347486404219,401.48018651652));
#4714=CARTESIAN_POINT('Ctrl Pts',(6.44230837852261,-189.773691234096,402.828149962177));
#4715=CARTESIAN_POINT('Ctrl Pts',(6.13076939848926,-189.353835745446,403.424338847606));
#4716=CARTESIAN_POINT('Ctrl Pts',(5.50080088534137,-188.411054784548,404.367119808505));
#4717=CARTESIAN_POINT('Ctrl Pts',(5.13065352868785,-187.815687292683,404.779503215329));
#4718=CARTESIAN_POINT('Ctrl Pts',(4.68703690659531,-186.81849775152,405.203220220576));
#4719=CARTESIAN_POINT('Ctrl Pts',(4.55888740591996,-186.468280486434,405.313196276448));
#4720=CARTESIAN_POINT('Ctrl Pts',(4.37998128622333,-185.746075739511,405.461618176925));
#4721=CARTESIAN_POINT('Ctrl Pts',(4.33012701892219,-185.37385187057,405.5));
#4722=CARTESIAN_POINT('Ctrl Pts',(4.33012701892219,-185.,405.5));
#4723=CARTESIAN_POINT('',(8.35164654424502,-185.,405.5));
#4724=CARTESIAN_POINT('',(-50.,-185.,405.5));
#4725=CARTESIAN_POINT('Ctrl Pts',(8.35164654424504,-185.,394.5));
#4726=CARTESIAN_POINT('Ctrl Pts',(8.35164654424504,-185.70976459468,394.5));
#4727=CARTESIAN_POINT('Ctrl Pts',(8.45174305106268,-186.452146928437,394.64504316336));
#4728=CARTESIAN_POINT('Ctrl Pts',(8.78438651561337,-187.800400830141,395.210212504666));
#4729=CARTESIAN_POINT('Ctrl Pts',(9.00975031605896,-188.408175830575,395.630001237523));
#4730=CARTESIAN_POINT('Ctrl Pts',(9.41491390301225,-189.367957849383,396.589783256331));
#4731=CARTESIAN_POINT('Ctrl Pts',(9.62434109787451,-189.789209811972,397.198189638843));
#4732=CARTESIAN_POINT('Ctrl Pts',(9.9183649900524,-190.355609616638,398.549441755203));
#4733=CARTESIAN_POINT('Ctrl Pts',(10.,-190.5,399.293247535323));
#4734=CARTESIAN_POINT('Ctrl Pts',(10.,-190.5,400.706752464677));
#4735=CARTESIAN_POINT('Ctrl Pts',(9.91836499005243,-190.355609616638,401.450558244797));
#4736=CARTESIAN_POINT('Ctrl Pts',(9.62434109787455,-189.789209811972,402.801810361157));
#4737=CARTESIAN_POINT('Ctrl Pts',(9.41491390301225,-189.367957849383,403.410216743669));
#4738=CARTESIAN_POINT('Ctrl Pts',(9.00975031605896,-188.408175830575,404.369998762477));
#4739=CARTESIAN_POINT('Ctrl Pts',(8.78438651561337,-187.800400830141,404.789787495334));
#4740=CARTESIAN_POINT('Ctrl Pts',(8.45174305106268,-186.452146928437,405.35495683664));
#4741=CARTESIAN_POINT('Ctrl Pts',(8.35164654424506,-185.70976459468,405.5));
#4742=CARTESIAN_POINT('Ctrl Pts',(8.35164654424506,-184.290235405321,405.5));
#4743=CARTESIAN_POINT('Ctrl Pts',(8.45174305106268,-183.547853071563,405.35495683664));
#4744=CARTESIAN_POINT('Ctrl Pts',(8.78438651561337,-182.199599169859,404.789787495334));
#4745=CARTESIAN_POINT('Ctrl Pts',(9.00975031605896,-181.591824169425,404.369998762477));
#4746=CARTESIAN_POINT('Ctrl Pts',(9.41491390301225,-180.632042150617,403.410216743669));
#4747=CARTESIAN_POINT('Ctrl Pts',(9.62434109787453,-180.210790188028,402.801810361157));
#4748=CARTESIAN_POINT('Ctrl Pts',(9.91836499005242,-179.644390383362,401.450558244797));
#4749=CARTESIAN_POINT('Ctrl Pts',(10.,-179.5,400.706752464677));
#4750=CARTESIAN_POINT('Ctrl Pts',(10.,-179.5,399.293247535323));
#4751=CARTESIAN_POINT('Ctrl Pts',(9.91836499005242,-179.644390383362,398.549441755203));
#4752=CARTESIAN_POINT('Ctrl Pts',(9.62434109787453,-180.210790188028,397.198189638843));
#4753=CARTESIAN_POINT('Ctrl Pts',(9.41491390301225,-180.632042150617,396.589783256331));
#4754=CARTESIAN_POINT('Ctrl Pts',(9.00975031605896,-181.591824169425,395.630001237523));
#4755=CARTESIAN_POINT('Ctrl Pts',(8.78438651561337,-182.199599169859,395.210212504666));
#4756=CARTESIAN_POINT('Ctrl Pts',(8.45174305106268,-183.547853071563,394.64504316336));
#4757=CARTESIAN_POINT('Ctrl Pts',(8.35164654424504,-184.290235405321,394.5));
#4758=CARTESIAN_POINT('Ctrl Pts',(8.35164654424504,-185.,394.5));
#4759=CARTESIAN_POINT('Ctrl Pts',(4.33012701892219,-185.,405.5));
#4760=CARTESIAN_POINT('Ctrl Pts',(4.33012701892219,-184.626148129431,405.5));
#4761=CARTESIAN_POINT('Ctrl Pts',(4.37998128622333,-184.25392426049,405.461618176925));
#4762=CARTESIAN_POINT('Ctrl Pts',(4.55888740591996,-183.531719513566,405.313196276448));
#4763=CARTESIAN_POINT('Ctrl Pts',(4.68703690659531,-183.18150224848,405.203220220576));
#4764=CARTESIAN_POINT('Ctrl Pts',(5.13065352868785,-182.184312707317,404.779503215329));
#4765=CARTESIAN_POINT('Ctrl Pts',(5.50080088534137,-181.588945215453,404.367119808505));
#4766=CARTESIAN_POINT('Ctrl Pts',(6.13076939848926,-180.646164254554,403.424338847606));
#4767=CARTESIAN_POINT('Ctrl Pts',(6.44230837852263,-180.226308765904,402.828149962177));
#4768=CARTESIAN_POINT('Ctrl Pts',(6.87828608217354,-179.652513595781,401.48018651652));
#4769=CARTESIAN_POINT('Ctrl Pts',(7.00000000000001,-179.5,400.726925774374));
#4770=CARTESIAN_POINT('Ctrl Pts',(7.00000000000001,-179.5,399.273074225626));
#4771=CARTESIAN_POINT('Ctrl Pts',(6.87828608217351,-179.652513595781,398.51981348348));
#4772=CARTESIAN_POINT('Ctrl Pts',(6.44230837852252,-180.226308765904,397.171850037822));
#4773=CARTESIAN_POINT('Ctrl Pts',(6.13076939848926,-180.646164254554,396.575661152394));
#4774=CARTESIAN_POINT('Ctrl Pts',(5.50080088534137,-181.588945215453,395.632880191495));
#4775=CARTESIAN_POINT('Ctrl Pts',(5.13065352868785,-182.184312707317,395.220496784671));
#4776=CARTESIAN_POINT('Ctrl Pts',(4.68703690659531,-183.18150224848,394.796779779424));
#4777=CARTESIAN_POINT('Ctrl Pts',(4.55888740591996,-183.531719513566,394.686803723552));
#4778=CARTESIAN_POINT('Ctrl Pts',(4.37998128622333,-184.25392426049,394.538381823075));
#4779=CARTESIAN_POINT('Ctrl Pts',(4.3301270189222,-184.626148129431,394.5));
#4780=CARTESIAN_POINT('Ctrl Pts',(4.3301270189222,-185.,394.5));
#4781=CARTESIAN_POINT('Origin',(-32.5,3.40419430537205E-13,10.));
#4782=CARTESIAN_POINT('',(-28.5,3.39929571817546E-13,10.));
#4783=CARTESIAN_POINT('Origin',(-32.5,3.40419430537205E-13,10.));
#4784=CARTESIAN_POINT('',(-28.5,3.39929571817546E-13,0.));
#4785=CARTESIAN_POINT('',(-28.5,3.39929571817546E-13,10.));
#4786=CARTESIAN_POINT('Origin',(-32.5,3.40419430537205E-13,0.));
#4787=CARTESIAN_POINT('Origin',(-2.26946287024804E-13,-32.5,10.));
#4788=CARTESIAN_POINT('',(3.99999999999977,-32.5,10.));
#4789=CARTESIAN_POINT('Origin',(-2.26946287024804E-13,-32.5,10.));
#4790=CARTESIAN_POINT('',(3.99999999999977,-32.5,0.));
#4791=CARTESIAN_POINT('',(3.99999999999977,-32.5,10.));
#4792=CARTESIAN_POINT('Origin',(-2.26946287024804E-13,-32.5,0.));
#4793=CARTESIAN_POINT('Origin',(32.5,-1.13473143512402E-13,10.));
#4794=CARTESIAN_POINT('',(36.5,-1.13963002232061E-13,10.));
#4795=CARTESIAN_POINT('Origin',(32.5,-1.13473143512402E-13,10.));
#4796=CARTESIAN_POINT('',(36.5,-1.13963002232061E-13,0.));
#4797=CARTESIAN_POINT('',(36.5,-1.13963002232061E-13,10.));
#4798=CARTESIAN_POINT('Origin',(32.5,-1.13473143512402E-13,0.));
#4799=CARTESIAN_POINT('Origin',(0.,32.5,10.));
#4800=CARTESIAN_POINT('',(4.00000000000001,32.5,10.));
#4801=CARTESIAN_POINT('Origin',(0.,32.5,10.));
#4802=CARTESIAN_POINT('',(4.00000000000001,32.5,0.));
#4803=CARTESIAN_POINT('',(4.00000000000001,32.5,10.));
#4804=CARTESIAN_POINT('Origin',(0.,32.5,0.));
#4805=CARTESIAN_POINT('Origin',(0.,-1.73472347597681E-14,10.));
#4806=CARTESIAN_POINT('',(50.,-2.34704687555048E-14,0.));
#4807=CARTESIAN_POINT('Origin',(0.,-1.73472347597681E-14,0.));
#4808=CARTESIAN_POINT('',(50.,-2.34704687555048E-14,10.));
#4809=CARTESIAN_POINT('',(50.,-2.34704687555048E-14,10.));
#4810=CARTESIAN_POINT('Origin',(0.,-1.73472347597681E-14,10.));
#4811=CARTESIAN_POINT('Origin',(0.,-1.73472347597681E-14,370.));
#4812=CARTESIAN_POINT('',(-8.57252759403147E-16,-7.,10.));
#4813=CARTESIAN_POINT('',(-8.57252759403147E-16,-7.00000000000002,370.));
#4814=CARTESIAN_POINT('Origin',(0.,-4.68844182696437E-16,10.));
#4815=CARTESIAN_POINT('Origin',(0.,-200.,400.));
#4816=CARTESIAN_POINT('',(-8.57252759403148E-16,-200.,393.));
#4817=CARTESIAN_POINT('Origin',(0.,-200.,400.));
#4818=CARTESIAN_POINT('',(-8.57252759403148E-16,-200.,393.));
#4819=CARTESIAN_POINT('Origin',(0.,-1.73472347597681E-14,370.));
#4820=CARTESIAN_POINT('',(-1.22464679914735E-15,-10.,10.));
#4821=CARTESIAN_POINT('Origin',(0.,-4.68844182696437E-16,10.));
#4822=CARTESIAN_POINT('',(-1.22464679914735E-15,-10.,370.));
#4823=CARTESIAN_POINT('Origin',(0.,-200.,400.));
#4824=CARTESIAN_POINT('',(-1.22464679914735E-15,-200.,390.));
#4825=CARTESIAN_POINT('',(-1.22464679914735E-15,-200.,390.));
#4826=CARTESIAN_POINT('Origin',(0.,-200.,400.));
#4827=CARTESIAN_POINT('Origin',(0.,-200.,400.));
#4828=CARTESIAN_POINT('Origin',(0.,-1.73472347597681E-14,10.));
#4829=CARTESIAN_POINT('Origin',(0.,-1.73472347597681E-14,10.));
#4830=CARTESIAN_POINT('Origin',(0.,-3.08148791101958E-30,0.));
#4831=CARTESIAN_POINT('',(0.,0.,0.));
#4832=CARTESIAN_POINT('Origin',(-80.,-100.,-1.54074395550979E-30));
#4833=CARTESIAN_POINT('',(-80.,-25.,-5.5));
#4834=CARTESIAN_POINT('Origin',(-80.,-25.,-1.54074395550979E-30));
#4835=CARTESIAN_POINT('',(-80.,-10.,-5.5));
#4836=CARTESIAN_POINT('',(-80.,-100.,-5.5));
#4837=CARTESIAN_POINT('Origin',(-80.,-10.,-1.54074395550979E-30));
#4838=CARTESIAN_POINT('Origin',(-80.,-100.,-1.54074395550979E-30));
#4839=CARTESIAN_POINT('',(-80.,10.,-5.5));
#4840=CARTESIAN_POINT('Origin',(-80.,10.,-1.54074395550979E-30));
#4841=CARTESIAN_POINT('',(-80.,25.,-5.5));
#4842=CARTESIAN_POINT('',(-80.,-100.,-5.5));
#4843=CARTESIAN_POINT('Origin',(-80.,25.,-1.54074395550979E-30));
#4844=CARTESIAN_POINT('Origin',(20.,0.,-6.12323399573677E-15));
#4845=CARTESIAN_POINT('',(7.54951656745106E-14,-4.28626379701574E-15,-35.));
#4846=CARTESIAN_POINT('Origin',(4.85722573273506E-14,0.,-2.16513759715961E-14));
#4847=CARTESIAN_POINT('',(20.0000000000001,-4.28626379701574E-15,-35.));
#4848=CARTESIAN_POINT('',(20.,-4.28626379701574E-15,-35.));
#4849=CARTESIAN_POINT('Origin',(20.,0.,-6.12323399573675E-15));
#4850=CARTESIAN_POINT('Ctrl Pts',(20.,0.,-2.32063937709169E-15));
#4851=CARTESIAN_POINT('Ctrl Pts',(20.,3.83568392226736E-15,-2.32063937709169E-15));
#4852=CARTESIAN_POINT('Ctrl Pts',(20.,3.83568392226736E-15,-6.15632329935905E-15));
#4853=CARTESIAN_POINT('Ctrl Pts',(20.,3.83568392226736E-15,-9.99200722162641E-15));
#4854=CARTESIAN_POINT('Ctrl Pts',(20.,0.,-9.99200722162641E-15));
#4855=CARTESIAN_POINT('Ctrl Pts',(20.,-3.83568392226736E-15,-9.99200722162641E-15));
#4856=CARTESIAN_POINT('Ctrl Pts',(20.,-3.83568392226736E-15,-6.15632329935905E-15));
#4857=CARTESIAN_POINT('Ctrl Pts',(20.,-3.83568392226736E-15,-2.32063937709169E-15));
#4858=CARTESIAN_POINT('Ctrl Pts',(20.,0.,-2.32063937709169E-15));
#4859=CARTESIAN_POINT('Ctrl Pts',(19.735608974744,0.,-17.3092179814268));
#4860=CARTESIAN_POINT('Ctrl Pts',(19.735608974744,-17.3092179814268,-17.3092179814268));
#4861=CARTESIAN_POINT('Ctrl Pts',(19.7356089747439,-17.3092179814268,-6.36159836822499E-15));
#4862=CARTESIAN_POINT('Ctrl Pts',(19.7356089747439,-17.3092179814268,17.3092179814268));
#4863=CARTESIAN_POINT('Ctrl Pts',(19.7356089747439,0.,17.3092179814268));
#4864=CARTESIAN_POINT('Ctrl Pts',(19.7356089747439,17.3092179814268,17.3092179814268));
#4865=CARTESIAN_POINT('Ctrl Pts',(19.7356089747439,17.3092179814268,-6.36159836822499E-15));
#4866=CARTESIAN_POINT('Ctrl Pts',(19.735608974744,17.3092179814268,-17.3092179814268));
#4867=CARTESIAN_POINT('Ctrl Pts',(19.735608974744,0.,-17.3092179814268));
#4868=CARTESIAN_POINT('Ctrl Pts',(11.433857869888,0.,-32.5));
#4869=CARTESIAN_POINT('Ctrl Pts',(11.433857869888,-32.5,-32.5));
#4870=CARTESIAN_POINT('Ctrl Pts',(11.433857869888,-32.5,-1.28071368584476E-14));
#4871=CARTESIAN_POINT('Ctrl Pts',(11.4338578698879,-32.5,32.5));
#4872=CARTESIAN_POINT('Ctrl Pts',(11.4338578698879,0.,32.5));
#4873=CARTESIAN_POINT('Ctrl Pts',(11.4338578698879,32.5,32.5));
#4874=CARTESIAN_POINT('Ctrl Pts',(11.433857869888,32.5,-1.28071368584476E-14));
#4875=CARTESIAN_POINT('Ctrl Pts',(11.433857869888,32.5,-32.5));
#4876=CARTESIAN_POINT('Ctrl Pts',(11.433857869888,0.,-32.5));
#4877=CARTESIAN_POINT('',(11.433857869888,3.9801020972289E-15,-32.5));
#4878=CARTESIAN_POINT('Origin',(11.433857869888,0.,-1.27740475548253E-14));
#4879=CARTESIAN_POINT('',(20.,0.,-6.12323399573677E-15));
#4880=CARTESIAN_POINT('Origin',(-49.9918354814302,1.30926481293404E-16,
1.06909585183706));
#4881=CARTESIAN_POINT('Origin',(20.,0.,-6.12323399573677E-15));
#4882=CARTESIAN_POINT('',(20.0000000000001,-3.9801020972289E-15,-32.5));
#4883=CARTESIAN_POINT('Origin',(20.,0.,-6.12323399573675E-15));
#4884=CARTESIAN_POINT('',(20.,-3.9801020972289E-15,-32.5));
#4885=CARTESIAN_POINT('Origin',(-80.,25.,-1.54074395550979E-30));
#4886=CARTESIAN_POINT('',(-84.4398801855672,-10.,-14.3278562226806));
#4887=CARTESIAN_POINT('',(-84.4398801855672,-10.,14.3278562226806));
#4888=CARTESIAN_POINT('Origin',(-80.,-10.,-1.54074395550979E-30));
#4889=CARTESIAN_POINT('',(-84.4398801855672,-25.,-14.3278562226806));
#4890=CARTESIAN_POINT('',(-84.4398801855672,25.,-14.3278562226806));
#4891=CARTESIAN_POINT('',(-84.4398801855672,-25.,14.3278562226806));
#4892=CARTESIAN_POINT('Origin',(-80.,-25.,-1.54074395550979E-30));
#4893=CARTESIAN_POINT('',(-84.4398801855672,25.,14.3278562226806));
#4894=CARTESIAN_POINT('Origin',(-84.4398801855672,25.,14.3278562226806));
#4895=CARTESIAN_POINT('',(-50.,-10.,25.));
#4896=CARTESIAN_POINT('',(-84.4398801855672,-10.,14.3278562226806));
#4897=CARTESIAN_POINT('',(-50.,-25.,25.));
#4898=CARTESIAN_POINT('',(-84.4398801855672,-25.,14.3278562226806));
#4899=CARTESIAN_POINT('',(-50.,25.,25.));
#4900=CARTESIAN_POINT('Origin',(-50.,25.,-25.));
#4901=CARTESIAN_POINT('',(-50.,-10.,-25.));
#4902=CARTESIAN_POINT('',(-50.,-10.,-25.));
#4903=CARTESIAN_POINT('',(-50.,-25.,-25.));
#4904=CARTESIAN_POINT('',(-50.,25.,-25.));
#4905=CARTESIAN_POINT('',(-50.,-25.,-25.));
#4906=CARTESIAN_POINT('Origin',(-50.,-80.,-30.));
#4907=CARTESIAN_POINT('',(0.,-100.,-30.));
#4908=CARTESIAN_POINT('',(0.,-80.,-50.));
#4909=CARTESIAN_POINT('Origin',(0.,-80.,-30.));
#4910=CARTESIAN_POINT('',(-50.,-100.,-30.));
#4911=CARTESIAN_POINT('',(-50.,-100.,-30.));
#4912=CARTESIAN_POINT('',(-50.,-80.,-50.));
#4913=CARTESIAN_POINT('Origin',(-50.,-80.,-30.));
#4914=CARTESIAN_POINT('',(-50.,-80.,-50.));
#4915=CARTESIAN_POINT('Origin',(-50.,-100.,-30.));
#4916=CARTESIAN_POINT('',(0.,-100.,30.));
#4917=CARTESIAN_POINT('',(0.,-100.,-30.));
#4918=CARTESIAN_POINT('',(-50.,-100.,30.));
#4919=CARTESIAN_POINT('',(-50.,-100.,30.));
#4920=CARTESIAN_POINT('',(-50.,-100.,-30.));
#4921=CARTESIAN_POINT('Origin',(-50.,-80.,30.));
#4922=CARTESIAN_POINT('',(0.,-80.,50.));
#4923=CARTESIAN_POINT('Origin',(0.,-80.,30.));
#4924=CARTESIAN_POINT('',(-50.,-80.,50.));
#4925=CARTESIAN_POINT('',(-50.,-80.,50.));
#4926=CARTESIAN_POINT('Origin',(-50.,-80.,30.));
#4927=CARTESIAN_POINT('Origin',(-50.,-80.,50.));
#4928=CARTESIAN_POINT('',(0.,80.,50.));
#4929=CARTESIAN_POINT('',(0.,-80.,50.));
#4930=CARTESIAN_POINT('',(-50.,80.,50.));
#4931=CARTESIAN_POINT('',(-50.,80.,50.));
#4932=CARTESIAN_POINT('',(-50.,-80.,50.));
#4933=CARTESIAN_POINT('Origin',(-50.,80.,30.));
#4934=CARTESIAN_POINT('',(0.,100.,30.));
#4935=CARTESIAN_POINT('Origin',(0.,80.,30.));
#4936=CARTESIAN_POINT('',(-50.,100.,30.));
#4937=CARTESIAN_POINT('',(-50.,100.,30.));
#4938=CARTESIAN_POINT('Origin',(-50.,80.,30.));
#4939=CARTESIAN_POINT('Origin',(-50.,100.,-30.));
#4940=CARTESIAN_POINT('',(0.,100.,-30.));
#4941=CARTESIAN_POINT('',(0.,100.,-30.));
#4942=CARTESIAN_POINT('',(-50.,100.,-30.));
#4943=CARTESIAN_POINT('',(-50.,100.,-30.));
#4944=CARTESIAN_POINT('',(-50.,100.,-30.));
#4945=CARTESIAN_POINT('Origin',(-50.,80.,-30.));
#4946=CARTESIAN_POINT('',(0.,80.,-50.));
#4947=CARTESIAN_POINT('Origin',(0.,80.,-30.));
#4948=CARTESIAN_POINT('',(-50.,80.,-50.));
#4949=CARTESIAN_POINT('',(-50.,80.,-50.));
#4950=CARTESIAN_POINT('Origin',(-50.,80.,-30.));
#4951=CARTESIAN_POINT('Origin',(-50.,-80.,-50.));
#4952=CARTESIAN_POINT('',(0.,-80.,-50.));
#4953=CARTESIAN_POINT('',(-50.,-80.,-50.));
#4954=CARTESIAN_POINT('Origin',(-50.,-80.,-30.));
#4955=CARTESIAN_POINT('',(-50.,25.,25.));
#4956=CARTESIAN_POINT('',(-50.,10.,25.));
#4957=CARTESIAN_POINT('',(-50.,25.,25.));
#4958=CARTESIAN_POINT('',(-50.,10.,-25.));
#4959=CARTESIAN_POINT('',(-50.,10.,25.));
#4960=CARTESIAN_POINT('',(-50.,25.,-25.));
#4961=CARTESIAN_POINT('',(-50.,25.,-25.));
#4962=CARTESIAN_POINT('',(-50.,25.,25.));
#4963=CARTESIAN_POINT('',(-50.,-10.,25.));
#4964=CARTESIAN_POINT('',(-50.,-25.,25.));
#4965=CARTESIAN_POINT('Origin',(0.,-80.,-30.));
#4966=CARTESIAN_POINT('Origin',(20.,0.,2.0344769428144E-29));
#4967=CARTESIAN_POINT('Origin',(-80.,25.,-1.54074395550979E-30));
#4968=CARTESIAN_POINT('',(-84.4398801855672,25.,-14.3278562226806));
#4969=CARTESIAN_POINT('',(-84.4398801855672,10.,-14.3278562226806));
#4970=CARTESIAN_POINT('',(-84.4398801855672,25.,-14.3278562226806));
#4971=CARTESIAN_POINT('',(-84.4398801855672,10.,14.3278562226806));
#4972=CARTESIAN_POINT('Origin',(-80.,10.,-1.54074395550979E-30));
#4973=CARTESIAN_POINT('',(-84.4398801855672,25.,14.3278562226806));
#4974=CARTESIAN_POINT('',(-84.4398801855672,25.,14.3278562226806));
#4975=CARTESIAN_POINT('Origin',(-80.,25.,-1.54074395550979E-30));
#4976=CARTESIAN_POINT('Origin',(-84.4398801855672,25.,14.3278562226806));
#4977=CARTESIAN_POINT('',(-84.4398801855672,10.,14.3278562226806));
#4978=CARTESIAN_POINT('',(-84.4398801855672,25.,14.3278562226806));
#4979=CARTESIAN_POINT('Origin',(-50.,25.,-25.));
#4980=CARTESIAN_POINT('',(-50.,10.,-25.));
#4981=CARTESIAN_POINT('',(-50.,25.,-25.));
#4982=CARTESIAN_POINT('Origin',(-80.,25.,-1.54074395550979E-30));
#4983=CARTESIAN_POINT('Origin',(-80.,-25.,-1.54074395550979E-30));
#4984=CARTESIAN_POINT('Origin',(-80.,-10.,-1.54074395550979E-30));
#4985=CARTESIAN_POINT('Origin',(-80.,10.,-1.54074395550979E-30));
#4986=CARTESIAN_POINT('',(0.,0.,0.));
#4987=CARTESIAN_POINT('Origin',(0.,0.,-25.0375057290932));
#4988=CARTESIAN_POINT('',(-5.,-6.12323399573677E-16,-8.4));
#4989=CARTESIAN_POINT('Origin',(0.,0.,-8.4));
#4990=CARTESIAN_POINT('',(-5.,-6.12323399573677E-16,0.));
#4991=CARTESIAN_POINT('',(-5.,-6.12323399573677E-16,-25.0375057290932));
#4992=CARTESIAN_POINT('Origin',(0.,0.,-3.25260651745651E-16));
#4993=CARTESIAN_POINT('Origin',(1.58955611655707E-15,9.23760430703403,-8.4));
#4994=CARTESIAN_POINT('',(-8.,4.61880215351705,-7.68546882018366));
#4995=CARTESIAN_POINT('',(-8.,4.61880215351699,-0.714531179816323));
#4996=CARTESIAN_POINT('',(-8.,4.61880215351699,-8.4));
#4997=CARTESIAN_POINT('',(-4.00000000000002,6.9282032302755,0.));
#4998=CARTESIAN_POINT('Ctrl Pts',(-8.00000000003847,4.61880215349478,-0.714531179829145));
#4999=CARTESIAN_POINT('Ctrl Pts',(-5.85640646056649,5.85640646054208,-8.88178419700125E-16));
#5000=CARTESIAN_POINT('Ctrl Pts',(-4.00000000000002,6.9282032302755,-8.80439423444571E-16));
#5001=CARTESIAN_POINT('',(-2.60208521396521E-15,9.23760430703403,-0.71453117981634));
#5002=CARTESIAN_POINT('Ctrl Pts',(-4.00000000000002,6.9282032302755,-8.80439423444571E-16));
#5003=CARTESIAN_POINT('Ctrl Pts',(-2.14359353943353,8.00000000000893,-8.83359324974957E-16));
#5004=CARTESIAN_POINT('Ctrl Pts',(3.84704779639695E-11,9.23760430705624,
-0.714531179829162));
#5005=CARTESIAN_POINT('',(8.67361737988404E-16,9.23760430703403,-7.68546882018366));
#5006=CARTESIAN_POINT('',(1.58955611655707E-15,9.23760430703403,-8.4));
#5007=CARTESIAN_POINT('',(-4.00000000000002,6.9282032302755,-8.4));
#5008=CARTESIAN_POINT('Ctrl Pts',(-4.00000000000004,6.92820323027549,-8.4));
#5009=CARTESIAN_POINT('Ctrl Pts',(-2.14359353943354,8.00000000000893,-8.4));
#5010=CARTESIAN_POINT('Ctrl Pts',(3.84766434846935E-11,9.23760430705625,
-7.68546882017083));
#5011=CARTESIAN_POINT('Ctrl Pts',(-8.00000000003847,4.61880215349478,-7.68546882017085));
#5012=CARTESIAN_POINT('Ctrl Pts',(-5.8564064605665,5.85640646054207,-8.4));
#5013=CARTESIAN_POINT('Ctrl Pts',(-4.00000000000004,6.92820323027549,-8.4));
#5014=CARTESIAN_POINT('Origin',(8.,4.61880215351698,-8.4));
#5015=CARTESIAN_POINT('',(4.00000000000003,6.92820323027549,0.));
#5016=CARTESIAN_POINT('Ctrl Pts',(-3.84662095265451E-11,9.23760430705625,
-0.714531179829163));
#5017=CARTESIAN_POINT('Ctrl Pts',(2.14359353943354,8.00000000000893,-6.66133814775094E-16));
#5018=CARTESIAN_POINT('Ctrl Pts',(4.00000000000003,6.9282032302755,-1.10054927930571E-15));
#5019=CARTESIAN_POINT('',(8.,4.61880215351705,-0.71453117981634));
#5020=CARTESIAN_POINT('Ctrl Pts',(4.00000000000003,6.9282032302755,-1.10054927930571E-15));
#5021=CARTESIAN_POINT('Ctrl Pts',(5.85640646056649,5.85640646054208,-1.85819040300646E-15));
#5022=CARTESIAN_POINT('Ctrl Pts',(8.00000000003845,4.61880215349479,-0.71453117982914));
#5023=CARTESIAN_POINT('',(8.,4.61880215351705,-7.68546882018366));
#5024=CARTESIAN_POINT('',(8.,4.61880215351698,-8.4));
#5025=CARTESIAN_POINT('',(4.00000000000003,6.92820323027549,-8.4));
#5026=CARTESIAN_POINT('Ctrl Pts',(4.00000000000004,6.92820323027549,-8.4));
#5027=CARTESIAN_POINT('Ctrl Pts',(5.85640646056649,5.85640646054208,-8.4));
#5028=CARTESIAN_POINT('Ctrl Pts',(8.00000000003844,4.61880215349479,-7.68546882017086));
#5029=CARTESIAN_POINT('Ctrl Pts',(-3.84676323390199E-11,9.23760430705624,
-7.68546882017084));
#5030=CARTESIAN_POINT('Ctrl Pts',(2.14359353943355,8.00000000000892,-8.4));
#5031=CARTESIAN_POINT('Ctrl Pts',(4.00000000000004,6.92820323027549,-8.4));
#5032=CARTESIAN_POINT('Origin',(8.,4.61880215351698,-8.4));
#5033=CARTESIAN_POINT('',(8.,-4.61880215351705,-0.71453117981634));
#5034=CARTESIAN_POINT('',(8.,0.,0.));
#5035=CARTESIAN_POINT('Ctrl Pts',(8.00000000000001,-4.61880215356147,-0.714531179829163));
#5036=CARTESIAN_POINT('Ctrl Pts',(8.00000000000001,-2.14359353946685,-3.88578058618805E-16));
#5037=CARTESIAN_POINT('Ctrl Pts',(8.,4.40219711722286E-15,-8.80439423444572E-16));
#5038=CARTESIAN_POINT('',(8.,-4.61880215351705,-7.68546882018366));
#5039=CARTESIAN_POINT('',(8.,-4.61880215351705,-8.4));
#5040=CARTESIAN_POINT('',(8.,0.,-8.4));
#5041=CARTESIAN_POINT('Ctrl Pts',(8.,-4.61880215356146,-7.68546882017084));
#5042=CARTESIAN_POINT('Ctrl Pts',(8.,-2.14359353946686,-8.4));
#5043=CARTESIAN_POINT('Ctrl Pts',(8.,-1.49674701985577E-14,-8.4));
#5044=CARTESIAN_POINT('Ctrl Pts',(8.,-1.49674701985577E-14,-8.4));
#5045=CARTESIAN_POINT('Ctrl Pts',(8.,2.14359353946684,-8.4));
#5046=CARTESIAN_POINT('Ctrl Pts',(8.,4.61880215356146,-7.68546882017084));
#5047=CARTESIAN_POINT('Ctrl Pts',(8.,-7.04351538755657E-15,4.40219711722283E-16));
#5048=CARTESIAN_POINT('Ctrl Pts',(8.,2.14359353946685,1.78210854566576E-15));
#5049=CARTESIAN_POINT('Ctrl Pts',(8.,4.61880215356148,-0.714531179829165));
#5050=CARTESIAN_POINT('Origin',(-3.00462919747434E-15,-9.23760430703408,
-8.4));
#5051=CARTESIAN_POINT('',(4.00000000000002,-6.9282032302755,0.));
#5052=CARTESIAN_POINT('Ctrl Pts',(8.00000000003846,-4.61880215349484,-0.714531179829161));
#5053=CARTESIAN_POINT('Ctrl Pts',(5.85640646056651,-5.85640646054213,-2.80331313717852E-14));
#5054=CARTESIAN_POINT('Ctrl Pts',(4.00000000000005,-6.92820323027554,-2.72936221267818E-14));
#5055=CARTESIAN_POINT('',(-8.93382590128056E-14,-9.23760430703403,-0.71453117981634));
#5056=CARTESIAN_POINT('Ctrl Pts',(4.00000000000005,-6.92820323027554,-2.72936221267818E-14));
#5057=CARTESIAN_POINT('Ctrl Pts',(2.14359353943354,-8.00000000000898,-2.65463710222373E-14));
#5058=CARTESIAN_POINT('Ctrl Pts',(-3.84861289011922E-11,-9.2376043070563,
-0.714531179829196));
#5059=CARTESIAN_POINT('',(-8.93382590128056E-14,-9.23760430703403,-7.68546882018366));
#5060=CARTESIAN_POINT('',(-3.00462919747434E-15,-9.23760430703408,-8.4));
#5061=CARTESIAN_POINT('',(4.00000000000002,-6.9282032302755,-8.4));
#5062=CARTESIAN_POINT('Ctrl Pts',(4.00000000000004,-6.92820323027554,-8.39999999999997));
#5063=CARTESIAN_POINT('Ctrl Pts',(2.14359353943353,-8.00000000000898,-8.39999999999997));
#5064=CARTESIAN_POINT('Ctrl Pts',(-3.85013055675899E-11,-9.23760430705631,
-7.6854688201708));
#5065=CARTESIAN_POINT('Ctrl Pts',(8.00000000003848,-4.61880215349483,-7.68546882017083));
#5066=CARTESIAN_POINT('Ctrl Pts',(5.85640646056651,-5.85640646054213,-8.39999999999997));
#5067=CARTESIAN_POINT('Ctrl Pts',(4.00000000000004,-6.92820323027554,-8.39999999999997));
#5068=CARTESIAN_POINT('Origin',(-8.,-4.61880215351704,-8.4));
#5069=CARTESIAN_POINT('',(-4.00000000000003,-6.92820323027549,0.));
#5070=CARTESIAN_POINT('Ctrl Pts',(3.83779951531087E-11,-9.23760430705625,
-0.714531179829162));
#5071=CARTESIAN_POINT('Ctrl Pts',(-2.14359353943358,-8.00000000000896,-2.75890421619351E-14));
#5072=CARTESIAN_POINT('Ctrl Pts',(-4.00000000000004,-6.92820323027554,-2.72936221267818E-14));
#5073=CARTESIAN_POINT('',(-8.,-4.61880215351705,-0.71453117981634));
#5074=CARTESIAN_POINT('Ctrl Pts',(-4.00000000000004,-6.92820323027554,-2.72936221267818E-14));
#5075=CARTESIAN_POINT('Ctrl Pts',(-5.8564064605665,-5.85640646054213,-2.68814782430319E-14));
#5076=CARTESIAN_POINT('Ctrl Pts',(-8.00000000003846,-4.61880215349484,-0.714531179829158));
#5077=CARTESIAN_POINT('',(-8.,-4.61880215351705,-7.68546882018366));
#5078=CARTESIAN_POINT('',(-8.,-4.61880215351704,-8.4));
#5079=CARTESIAN_POINT('',(-4.00000000000003,-6.92820323027549,-8.4));
#5080=CARTESIAN_POINT('Ctrl Pts',(-4.00000000000003,-6.92820323027555,-8.39999999999998));
#5081=CARTESIAN_POINT('Ctrl Pts',(-5.8564064605665,-5.85640646054213,-8.39999999999998));
#5082=CARTESIAN_POINT('Ctrl Pts',(-8.00000000003846,-4.61880215349483,-7.68546882017084));
#5083=CARTESIAN_POINT('Ctrl Pts',(3.83836864030079E-11,-9.23760430705625,
-7.68546882017084));
#5084=CARTESIAN_POINT('Ctrl Pts',(-2.14359353943357,-8.00000000000896,-8.39999999999997));
#5085=CARTESIAN_POINT('Ctrl Pts',(-4.00000000000003,-6.92820323027555,-8.39999999999998));
#5086=CARTESIAN_POINT('Origin',(-8.,4.61880215351699,-8.4));
#5087=CARTESIAN_POINT('',(-8.,0.,0.));
#5088=CARTESIAN_POINT('Ctrl Pts',(-8.00000000000001,-4.61880215356147,-0.714531179829163));
#5089=CARTESIAN_POINT('Ctrl Pts',(-8.00000000000001,-2.14359353946685,-3.88578058618805E-16));
#5090=CARTESIAN_POINT('Ctrl Pts',(-8.,4.40219711722286E-15,-8.80439423444572E-16));
#5091=CARTESIAN_POINT('Ctrl Pts',(-8.,4.40219711722286E-15,-8.80439423444572E-16));
#5092=CARTESIAN_POINT('Ctrl Pts',(-8.,2.14359353946683,-1.72112737696137E-15));
#5093=CARTESIAN_POINT('Ctrl Pts',(-8.00000000000001,4.61880215356141,-0.714531179829147));
#5094=CARTESIAN_POINT('',(-8.,0.,-8.4));
#5095=CARTESIAN_POINT('Ctrl Pts',(-8.,-1.49674701985577E-14,-8.4));
#5096=CARTESIAN_POINT('Ctrl Pts',(-8.,2.14359353946684,-8.4));
#5097=CARTESIAN_POINT('Ctrl Pts',(-8.,4.61880215356146,-7.68546882017084));
#5098=CARTESIAN_POINT('Ctrl Pts',(-8.,-4.61880215356146,-7.68546882017084));
#5099=CARTESIAN_POINT('Ctrl Pts',(-8.,-2.14359353946686,-8.4));
#5100=CARTESIAN_POINT('Ctrl Pts',(-8.,-1.49674701985577E-14,-8.4));
#5101=CARTESIAN_POINT('Origin',(-1.73472347597681E-15,9.23760430703403,
0.));
#5102=CARTESIAN_POINT('Origin',(0.,0.,0.));
#5103=CARTESIAN_POINT('Origin',(0.,0.,0.));
#5104=CARTESIAN_POINT('Origin',(0.,0.,0.));
#5105=CARTESIAN_POINT('Origin',(0.,0.,0.));
#5106=CARTESIAN_POINT('Origin',(0.,0.,0.));
#5107=CARTESIAN_POINT('Origin',(0.,0.,0.));
#5108=CARTESIAN_POINT('Origin',(-1.73472347597681E-15,9.23760430703403,
-8.4));
#5109=CARTESIAN_POINT('Origin',(0.,0.,-8.4));
#5110=CARTESIAN_POINT('Origin',(0.,0.,-8.4));
#5111=CARTESIAN_POINT('Origin',(0.,0.,-8.4));
#5112=CARTESIAN_POINT('Origin',(0.,0.,-8.4));
#5113=CARTESIAN_POINT('Origin',(0.,0.,-8.4));
#5114=CARTESIAN_POINT('Origin',(0.,0.,-8.4));
#5115=CARTESIAN_POINT('Origin',(0.,0.,-8.4));
#5116=CARTESIAN_POINT('Origin',(0.,0.,-8.4));
#5117=CARTESIAN_POINT('Origin',(0.,0.,-8.4));
#5118=CARTESIAN_POINT('Origin',(0.,0.,-8.4));
#5119=CARTESIAN_POINT('Origin',(0.,0.,-8.4));
#5120=CARTESIAN_POINT('Origin',(0.,0.,-8.4));
#5121=CARTESIAN_POINT('Origin',(0.,0.,0.));
#5122=CARTESIAN_POINT('Origin',(0.,0.,0.));
#5123=CARTESIAN_POINT('Origin',(0.,0.,0.));
#5124=CARTESIAN_POINT('Origin',(0.,0.,0.));
#5125=CARTESIAN_POINT('Origin',(0.,0.,0.));
#5126=CARTESIAN_POINT('Origin',(0.,0.,0.));
#5127=CARTESIAN_POINT('',(0.,0.,0.));
#5128=CARTESIAN_POINT('Origin',(0.,0.,-25.0375057290932));
#5129=CARTESIAN_POINT('',(-5.,-6.12323399573677E-16,-8.4));
#5130=CARTESIAN_POINT('Origin',(0.,0.,-8.4));
#5131=CARTESIAN_POINT('',(-5.,-6.12323399573677E-16,0.));
#5132=CARTESIAN_POINT('',(-5.,-6.12323399573677E-16,-25.0375057290932));
#5133=CARTESIAN_POINT('Origin',(0.,0.,3.25260651745651E-16));
#5134=CARTESIAN_POINT('Origin',(1.58955611655707E-15,9.23760430703403,-8.4));
#5135=CARTESIAN_POINT('',(-8.,4.61880215351705,-7.68546882018366));
#5136=CARTESIAN_POINT('',(-8.,4.61880215351699,-0.714531179816323));
#5137=CARTESIAN_POINT('',(-8.,4.61880215351699,-8.4));
#5138=CARTESIAN_POINT('',(-4.00000000000002,6.9282032302755,0.));
#5139=CARTESIAN_POINT('Ctrl Pts',(-8.00000000003847,4.61880215349478,-0.714531179829145));
#5140=CARTESIAN_POINT('Ctrl Pts',(-5.85640646056649,5.85640646054208,-8.88178419700125E-16));
#5141=CARTESIAN_POINT('Ctrl Pts',(-4.00000000000002,6.9282032302755,-8.80439423444571E-16));
#5142=CARTESIAN_POINT('',(-2.60208521396521E-15,9.23760430703403,-0.71453117981634));
#5143=CARTESIAN_POINT('Ctrl Pts',(-4.00000000000002,6.9282032302755,-8.80439423444571E-16));
#5144=CARTESIAN_POINT('Ctrl Pts',(-2.14359353943353,8.00000000000893,-8.83359324974957E-16));
#5145=CARTESIAN_POINT('Ctrl Pts',(3.84704779639695E-11,9.23760430705624,
-0.714531179829162));
#5146=CARTESIAN_POINT('',(8.67361737988404E-16,9.23760430703403,-7.68546882018366));
#5147=CARTESIAN_POINT('',(1.58955611655707E-15,9.23760430703403,-8.4));
#5148=CARTESIAN_POINT('',(-4.00000000000002,6.9282032302755,-8.4));
#5149=CARTESIAN_POINT('Ctrl Pts',(-4.00000000000004,6.92820323027549,-8.4));
#5150=CARTESIAN_POINT('Ctrl Pts',(-2.14359353943354,8.00000000000893,-8.4));
#5151=CARTESIAN_POINT('Ctrl Pts',(3.84766434846935E-11,9.23760430705625,
-7.68546882017083));
#5152=CARTESIAN_POINT('Ctrl Pts',(-8.00000000003847,4.61880215349478,-7.68546882017085));
#5153=CARTESIAN_POINT('Ctrl Pts',(-5.8564064605665,5.85640646054207,-8.4));
#5154=CARTESIAN_POINT('Ctrl Pts',(-4.00000000000004,6.92820323027549,-8.4));
#5155=CARTESIAN_POINT('Origin',(8.,4.61880215351698,-8.4));
#5156=CARTESIAN_POINT('',(4.00000000000003,6.92820323027549,0.));
#5157=CARTESIAN_POINT('Ctrl Pts',(-3.84662095265451E-11,9.23760430705625,
-0.714531179829163));
#5158=CARTESIAN_POINT('Ctrl Pts',(2.14359353943354,8.00000000000893,-6.66133814775094E-16));
#5159=CARTESIAN_POINT('Ctrl Pts',(4.00000000000003,6.9282032302755,-1.10054927930571E-15));
#5160=CARTESIAN_POINT('',(8.,4.61880215351705,-0.71453117981634));
#5161=CARTESIAN_POINT('Ctrl Pts',(4.00000000000003,6.9282032302755,-1.10054927930571E-15));
#5162=CARTESIAN_POINT('Ctrl Pts',(5.85640646056649,5.85640646054208,-1.85819040300646E-15));
#5163=CARTESIAN_POINT('Ctrl Pts',(8.00000000003845,4.61880215349479,-0.71453117982914));
#5164=CARTESIAN_POINT('',(8.,4.61880215351705,-7.68546882018366));
#5165=CARTESIAN_POINT('',(8.,4.61880215351698,-8.4));
#5166=CARTESIAN_POINT('',(4.00000000000003,6.92820323027549,-8.4));
#5167=CARTESIAN_POINT('Ctrl Pts',(4.00000000000004,6.92820323027549,-8.4));
#5168=CARTESIAN_POINT('Ctrl Pts',(5.85640646056649,5.85640646054208,-8.4));
#5169=CARTESIAN_POINT('Ctrl Pts',(8.00000000003844,4.61880215349479,-7.68546882017086));
#5170=CARTESIAN_POINT('Ctrl Pts',(-3.84676323390199E-11,9.23760430705624,
-7.68546882017084));
#5171=CARTESIAN_POINT('Ctrl Pts',(2.14359353943355,8.00000000000892,-8.4));
#5172=CARTESIAN_POINT('Ctrl Pts',(4.00000000000004,6.92820323027549,-8.4));
#5173=CARTESIAN_POINT('Origin',(8.,4.61880215351698,-8.4));
#5174=CARTESIAN_POINT('',(8.,-4.61880215351705,-0.71453117981634));
#5175=CARTESIAN_POINT('',(8.,0.,0.));
#5176=CARTESIAN_POINT('Ctrl Pts',(8.00000000000001,-4.61880215356147,-0.714531179829163));
#5177=CARTESIAN_POINT('Ctrl Pts',(8.00000000000001,-2.14359353946685,-3.88578058618805E-16));
#5178=CARTESIAN_POINT('Ctrl Pts',(8.,4.40219711722286E-15,-8.80439423444572E-16));
#5179=CARTESIAN_POINT('',(8.,-4.61880215351705,-7.68546882018366));
#5180=CARTESIAN_POINT('',(8.,-4.61880215351705,-8.4));
#5181=CARTESIAN_POINT('',(8.,0.,-8.4));
#5182=CARTESIAN_POINT('Ctrl Pts',(8.,-4.61880215356146,-7.68546882017084));
#5183=CARTESIAN_POINT('Ctrl Pts',(8.,-2.14359353946686,-8.4));
#5184=CARTESIAN_POINT('Ctrl Pts',(8.,-1.49674701985577E-14,-8.4));
#5185=CARTESIAN_POINT('Ctrl Pts',(8.,-1.49674701985577E-14,-8.4));
#5186=CARTESIAN_POINT('Ctrl Pts',(8.,2.14359353946684,-8.4));
#5187=CARTESIAN_POINT('Ctrl Pts',(8.,4.61880215356146,-7.68546882017084));
#5188=CARTESIAN_POINT('Ctrl Pts',(8.,-7.04351538755657E-15,4.40219711722283E-16));
#5189=CARTESIAN_POINT('Ctrl Pts',(8.,2.14359353946685,1.78210854566576E-15));
#5190=CARTESIAN_POINT('Ctrl Pts',(8.,4.61880215356148,-0.714531179829165));
#5191=CARTESIAN_POINT('Origin',(-3.00462919747434E-15,-9.23760430703408,
-8.4));
#5192=CARTESIAN_POINT('',(4.00000000000002,-6.9282032302755,0.));
#5193=CARTESIAN_POINT('Ctrl Pts',(8.00000000003846,-4.61880215349484,-0.714531179829161));
#5194=CARTESIAN_POINT('Ctrl Pts',(5.85640646056651,-5.85640646054213,-2.80331313717852E-14));
#5195=CARTESIAN_POINT('Ctrl Pts',(4.00000000000005,-6.92820323027554,-2.72936221267818E-14));
#5196=CARTESIAN_POINT('',(-8.93382590128056E-14,-9.23760430703403,-0.71453117981634));
#5197=CARTESIAN_POINT('Ctrl Pts',(4.00000000000005,-6.92820323027554,-2.72936221267818E-14));
#5198=CARTESIAN_POINT('Ctrl Pts',(2.14359353943354,-8.00000000000898,-2.65463710222373E-14));
#5199=CARTESIAN_POINT('Ctrl Pts',(-3.84861289011922E-11,-9.2376043070563,
-0.714531179829196));
#5200=CARTESIAN_POINT('',(-8.93382590128056E-14,-9.23760430703403,-7.68546882018366));
#5201=CARTESIAN_POINT('',(-3.00462919747434E-15,-9.23760430703408,-8.4));
#5202=CARTESIAN_POINT('',(4.00000000000002,-6.9282032302755,-8.4));
#5203=CARTESIAN_POINT('Ctrl Pts',(4.00000000000004,-6.92820323027554,-8.39999999999997));
#5204=CARTESIAN_POINT('Ctrl Pts',(2.14359353943353,-8.00000000000898,-8.39999999999997));
#5205=CARTESIAN_POINT('Ctrl Pts',(-3.85013055675899E-11,-9.23760430705631,
-7.6854688201708));
#5206=CARTESIAN_POINT('Ctrl Pts',(8.00000000003848,-4.61880215349483,-7.68546882017083));
#5207=CARTESIAN_POINT('Ctrl Pts',(5.85640646056651,-5.85640646054213,-8.39999999999997));
#5208=CARTESIAN_POINT('Ctrl Pts',(4.00000000000004,-6.92820323027554,-8.39999999999997));
#5209=CARTESIAN_POINT('Origin',(-8.,-4.61880215351704,-8.4));
#5210=CARTESIAN_POINT('',(-4.00000000000003,-6.92820323027549,0.));
#5211=CARTESIAN_POINT('Ctrl Pts',(3.83779951531087E-11,-9.23760430705625,
-0.714531179829162));
#5212=CARTESIAN_POINT('Ctrl Pts',(-2.14359353943358,-8.00000000000896,-2.75890421619351E-14));
#5213=CARTESIAN_POINT('Ctrl Pts',(-4.00000000000004,-6.92820323027554,-2.72936221267818E-14));
#5214=CARTESIAN_POINT('',(-8.,-4.61880215351705,-0.71453117981634));
#5215=CARTESIAN_POINT('Ctrl Pts',(-4.00000000000004,-6.92820323027554,-2.72936221267818E-14));
#5216=CARTESIAN_POINT('Ctrl Pts',(-5.8564064605665,-5.85640646054213,-2.68814782430319E-14));
#5217=CARTESIAN_POINT('Ctrl Pts',(-8.00000000003846,-4.61880215349484,-0.714531179829158));
#5218=CARTESIAN_POINT('',(-8.,-4.61880215351705,-7.68546882018366));
#5219=CARTESIAN_POINT('',(-8.,-4.61880215351704,-8.4));
#5220=CARTESIAN_POINT('',(-4.00000000000003,-6.92820323027549,-8.4));
#5221=CARTESIAN_POINT('Ctrl Pts',(-4.00000000000003,-6.92820323027555,-8.39999999999998));
#5222=CARTESIAN_POINT('Ctrl Pts',(-5.8564064605665,-5.85640646054213,-8.39999999999998));
#5223=CARTESIAN_POINT('Ctrl Pts',(-8.00000000003846,-4.61880215349483,-7.68546882017084));
#5224=CARTESIAN_POINT('Ctrl Pts',(3.83836864030079E-11,-9.23760430705625,
-7.68546882017084));
#5225=CARTESIAN_POINT('Ctrl Pts',(-2.14359353943357,-8.00000000000896,-8.39999999999997));
#5226=CARTESIAN_POINT('Ctrl Pts',(-4.00000000000003,-6.92820323027555,-8.39999999999998));
#5227=CARTESIAN_POINT('Origin',(-8.,4.61880215351699,-8.4));
#5228=CARTESIAN_POINT('',(-8.,0.,0.));
#5229=CARTESIAN_POINT('Ctrl Pts',(-8.00000000000001,-4.61880215356147,-0.714531179829163));
#5230=CARTESIAN_POINT('Ctrl Pts',(-8.00000000000001,-2.14359353946685,-3.88578058618805E-16));
#5231=CARTESIAN_POINT('Ctrl Pts',(-8.,4.40219711722286E-15,-8.80439423444572E-16));
#5232=CARTESIAN_POINT('Ctrl Pts',(-8.,4.40219711722286E-15,-8.80439423444572E-16));
#5233=CARTESIAN_POINT('Ctrl Pts',(-8.,2.14359353946683,-1.72112737696137E-15));
#5234=CARTESIAN_POINT('Ctrl Pts',(-8.00000000000001,4.61880215356141,-0.714531179829147));
#5235=CARTESIAN_POINT('',(-8.,0.,-8.4));
#5236=CARTESIAN_POINT('Ctrl Pts',(-8.,-1.49674701985577E-14,-8.4));
#5237=CARTESIAN_POINT('Ctrl Pts',(-8.,2.14359353946684,-8.4));
#5238=CARTESIAN_POINT('Ctrl Pts',(-8.,4.61880215356146,-7.68546882017084));
#5239=CARTESIAN_POINT('Ctrl Pts',(-8.,-4.61880215356146,-7.68546882017084));
#5240=CARTESIAN_POINT('Ctrl Pts',(-8.,-2.14359353946686,-8.4));
#5241=CARTESIAN_POINT('Ctrl Pts',(-8.,-1.49674701985577E-14,-8.4));
#5242=CARTESIAN_POINT('Origin',(-1.73472347597681E-15,9.23760430703403,
0.));
#5243=CARTESIAN_POINT('Origin',(0.,0.,0.));
#5244=CARTESIAN_POINT('Origin',(0.,0.,0.));
#5245=CARTESIAN_POINT('Origin',(0.,0.,0.));
#5246=CARTESIAN_POINT('Origin',(0.,0.,0.));
#5247=CARTESIAN_POINT('Origin',(0.,0.,0.));
#5248=CARTESIAN_POINT('Origin',(0.,0.,0.));
#5249=CARTESIAN_POINT('Origin',(-1.73472347597681E-15,9.23760430703403,
-8.4));
#5250=CARTESIAN_POINT('Origin',(0.,0.,-8.4));
#5251=CARTESIAN_POINT('Origin',(0.,0.,-8.4));
#5252=CARTESIAN_POINT('Origin',(0.,0.,-8.4));
#5253=CARTESIAN_POINT('Origin',(0.,0.,-8.4));
#5254=CARTESIAN_POINT('Origin',(0.,0.,-8.4));
#5255=CARTESIAN_POINT('Origin',(0.,0.,-8.4));
#5256=CARTESIAN_POINT('Origin',(0.,0.,-8.4));
#5257=CARTESIAN_POINT('Origin',(0.,0.,-8.4));
#5258=CARTESIAN_POINT('Origin',(0.,0.,-8.4));
#5259=CARTESIAN_POINT('Origin',(0.,0.,-8.4));
#5260=CARTESIAN_POINT('Origin',(0.,0.,-8.4));
#5261=CARTESIAN_POINT('Origin',(0.,0.,-8.4));
#5262=CARTESIAN_POINT('Origin',(0.,0.,0.));
#5263=CARTESIAN_POINT('Origin',(0.,0.,0.));
#5264=CARTESIAN_POINT('Origin',(0.,0.,0.));
#5265=CARTESIAN_POINT('Origin',(0.,0.,0.));
#5266=CARTESIAN_POINT('Origin',(0.,0.,0.));
#5267=CARTESIAN_POINT('Origin',(0.,0.,0.));
#5268=CARTESIAN_POINT('',(0.,0.,0.));
#5269=CARTESIAN_POINT('Origin',(0.,30.,-50.));
#5270=CARTESIAN_POINT('',(-5.,30.,-50.));
#5271=CARTESIAN_POINT('Origin',(0.,30.,-50.));
#5272=CARTESIAN_POINT('',(-5.,30.,-45.));
#5273=CARTESIAN_POINT('',(-5.,30.,-50.));
#5274=CARTESIAN_POINT('Origin',(0.,30.,-45.));
#5275=CARTESIAN_POINT('Origin',(0.,-30.,-50.));
#5276=CARTESIAN_POINT('',(-5.,-30.,-50.));
#5277=CARTESIAN_POINT('Origin',(0.,-30.,-50.));
#5278=CARTESIAN_POINT('',(-5.,-30.,-45.));
#5279=CARTESIAN_POINT('',(-5.,-30.,-50.));
#5280=CARTESIAN_POINT('Origin',(0.,-30.,-45.));
#5281=CARTESIAN_POINT('Origin',(0.,30.,-50.));
#5282=CARTESIAN_POINT('',(-5.,30.,45.));
#5283=CARTESIAN_POINT('Origin',(0.,30.,45.));
#5284=CARTESIAN_POINT('',(-5.,30.,50.));
#5285=CARTESIAN_POINT('',(-5.,30.,-50.));
#5286=CARTESIAN_POINT('Origin',(0.,30.,50.));
#5287=CARTESIAN_POINT('Origin',(0.,-30.,-50.));
#5288=CARTESIAN_POINT('',(-5.,-30.,45.));
#5289=CARTESIAN_POINT('Origin',(0.,-30.,45.));
#5290=CARTESIAN_POINT('',(-5.,-30.,50.));
#5291=CARTESIAN_POINT('',(-5.,-30.,-50.));
#5292=CARTESIAN_POINT('Origin',(0.,-30.,50.));
#5293=CARTESIAN_POINT('Origin',(-50.,-425.,3.46944695195361E-15));
#5294=CARTESIAN_POINT('',(45.,-425.,25.));
#5295=CARTESIAN_POINT('Origin',(45.,-425.,-3.12250225675825E-15));
#5296=CARTESIAN_POINT('',(50.,-425.,25.));
#5297=CARTESIAN_POINT('',(-50.,-425.,25.));
#5298=CARTESIAN_POINT('Origin',(50.,-425.,-3.46944695195361E-15));
#5299=CARTESIAN_POINT('Origin',(-50.,425.,3.46944695195361E-15));
#5300=CARTESIAN_POINT('',(45.,425.,25.));
#5301=CARTESIAN_POINT('Origin',(45.,425.,-3.12250225675825E-15));
#5302=CARTESIAN_POINT('',(50.,425.,25.));
#5303=CARTESIAN_POINT('',(-50.,425.,25.));
#5304=CARTESIAN_POINT('Origin',(50.,425.,-3.46944695195361E-15));
#5305=CARTESIAN_POINT('Origin',(-50.,-425.,3.46944695195361E-15));
#5306=CARTESIAN_POINT('',(-50.,-425.,25.));
#5307=CARTESIAN_POINT('Origin',(-50.,-425.,3.46944695195361E-15));
#5308=CARTESIAN_POINT('',(-45.,-425.,25.));
#5309=CARTESIAN_POINT('',(-50.,-425.,25.));
#5310=CARTESIAN_POINT('Origin',(-45.,-425.,3.12250225675825E-15));
#5311=CARTESIAN_POINT('Origin',(-50.,425.,3.46944695195361E-15));
#5312=CARTESIAN_POINT('',(-50.,425.,25.));
#5313=CARTESIAN_POINT('Origin',(-50.,425.,3.46944695195361E-15));
#5314=CARTESIAN_POINT('',(-45.,425.,25.));
#5315=CARTESIAN_POINT('',(-50.,425.,25.));
#5316=CARTESIAN_POINT('Origin',(-45.,425.,3.12250225675825E-15));
#5317=CARTESIAN_POINT('Origin',(0.,500.,0.));
#5318=CARTESIAN_POINT('',(50.,500.,50.));
#5319=CARTESIAN_POINT('',(50.,500.,-50.));
#5320=CARTESIAN_POINT('',(50.,500.,50.));
#5321=CARTESIAN_POINT('',(-50.,500.,-50.));
#5322=CARTESIAN_POINT('',(50.,500.,-50.));
#5323=CARTESIAN_POINT('',(-50.,500.,50.));
#5324=CARTESIAN_POINT('',(-50.,500.,50.));
#5325=CARTESIAN_POINT('',(50.,500.,50.));
#5326=CARTESIAN_POINT('',(45.,500.,-45.));
#5327=CARTESIAN_POINT('',(-45.,500.,-45.));
#5328=CARTESIAN_POINT('',(50.,500.,-45.));
#5329=CARTESIAN_POINT('',(45.,500.,45.));
#5330=CARTESIAN_POINT('',(45.,500.,50.));
#5331=CARTESIAN_POINT('',(-45.,500.,45.));
#5332=CARTESIAN_POINT('',(50.,500.,45.));
#5333=CARTESIAN_POINT('',(-45.,500.,50.));
#5334=CARTESIAN_POINT('Origin',(0.,-500.,0.));
#5335=CARTESIAN_POINT('',(50.,-500.,50.));
#5336=CARTESIAN_POINT('',(50.,-500.,-50.));
#5337=CARTESIAN_POINT('',(50.,-500.,50.));
#5338=CARTESIAN_POINT('',(-50.,-500.,50.));
#5339=CARTESIAN_POINT('',(50.,-500.,50.));
#5340=CARTESIAN_POINT('',(-50.,-500.,-50.));
#5341=CARTESIAN_POINT('',(-50.,-500.,50.));
#5342=CARTESIAN_POINT('',(50.,-500.,-50.));
#5343=CARTESIAN_POINT('',(45.,-500.,45.));
#5344=CARTESIAN_POINT('',(45.,-500.,-45.));
#5345=CARTESIAN_POINT('',(45.,-500.,50.));
#5346=CARTESIAN_POINT('',(-45.,-500.,-45.));
#5347=CARTESIAN_POINT('',(50.,-500.,-45.));
#5348=CARTESIAN_POINT('',(-45.,-500.,45.));
#5349=CARTESIAN_POINT('',(-45.,-500.,50.));
#5350=CARTESIAN_POINT('',(50.,-500.,45.));
#5351=CARTESIAN_POINT('Origin',(50.,500.,50.));
#5352=CARTESIAN_POINT('',(50.,500.,-50.));
#5353=CARTESIAN_POINT('',(50.,500.,50.));
#5354=CARTESIAN_POINT('Origin',(50.,500.,-50.));
#5355=CARTESIAN_POINT('',(-50.,500.,-50.));
#5356=CARTESIAN_POINT('Origin',(-50.,500.,50.));
#5357=CARTESIAN_POINT('',(-50.,500.,50.));
#5358=CARTESIAN_POINT('Origin',(50.,500.,50.));
#5359=CARTESIAN_POINT('Origin',(45.,500.,50.));
#5360=CARTESIAN_POINT('',(45.,500.,45.));
#5361=CARTESIAN_POINT('',(45.,500.,-45.));
#5362=CARTESIAN_POINT('Origin',(50.,500.,-45.));
#5363=CARTESIAN_POINT('',(-45.,500.,-45.));
#5364=CARTESIAN_POINT('Origin',(-45.,500.,50.));
#5365=CARTESIAN_POINT('',(-45.,500.,45.));
#5366=CARTESIAN_POINT('Origin',(50.,500.,45.));
#5367=CARTESIAN_POINT('',(0.,0.,0.));
#5368=CARTESIAN_POINT('Origin',(0.,300.,-2.77555756156289E-14));
#5369=CARTESIAN_POINT('',(9.18485099360515E-15,295.,-75.0000000000001));
#5370=CARTESIAN_POINT('',(-9.18485099360515E-15,295.,75.));
#5371=CARTESIAN_POINT('Origin',(0.,295.,-2.77555756156289E-14));
#5372=CARTESIAN_POINT('Origin',(0.,295.,-2.77555756156289E-14));
#5373=CARTESIAN_POINT('',(-8.57252759403148E-15,300.,70.));
#5374=CARTESIAN_POINT('',(-8.57252759403148E-15,300.,70.));
#5375=CARTESIAN_POINT('Origin',(0.,300.,-2.77555756156289E-14));
#5376=CARTESIAN_POINT('Origin',(0.,415.,-2.77555756156289E-14));
#5377=CARTESIAN_POINT('',(3.00038465791101E-15,410.,-24.5));
#5378=CARTESIAN_POINT('',(-3.00038465791101E-15,410.,24.5));
#5379=CARTESIAN_POINT('Origin',(0.,410.,-2.77555756156289E-14));
#5380=CARTESIAN_POINT('Origin',(0.,410.,-2.77555756156289E-14));
#5381=CARTESIAN_POINT('',(-2.38806125833733E-15,415.,19.4999999999999));
#5382=CARTESIAN_POINT('',(-2.38806125833733E-15,415.,19.4999999999999));
#5383=CARTESIAN_POINT('Origin',(0.,415.,-2.77555756156289E-14));
#5384=CARTESIAN_POINT('Origin',(0.,-410.,-2.77555756156289E-14));
#5385=CARTESIAN_POINT('',(-3.00038465791101E-15,-410.,-24.5));
#5386=CARTESIAN_POINT('Origin',(0.,-410.,-2.77555756156289E-14));
#5387=CARTESIAN_POINT('',(-2.38806125833733E-15,-415.,-19.5));
#5388=CARTESIAN_POINT('',(-3.00038465791101E-15,-410.,-24.5));
#5389=CARTESIAN_POINT('Origin',(0.,-415.,-2.77555756156289E-14));
#5390=CARTESIAN_POINT('Origin',(0.,-295.,-2.77555756156289E-14));
#5391=CARTESIAN_POINT('',(-9.18485099360515E-15,-295.,-75.0000000000001));
#5392=CARTESIAN_POINT('Origin',(0.,-295.,-2.77555756156289E-14));
#5393=CARTESIAN_POINT('',(-8.57252759403147E-15,-300.,-70.));
#5394=CARTESIAN_POINT('',(-9.18485099360515E-15,-295.,-75.0000000000001));
#5395=CARTESIAN_POINT('Origin',(0.,-300.,-2.77555756156289E-14));
#5396=CARTESIAN_POINT('Origin',(0.,-300.,-2.77555756156289E-14));
#5397=CARTESIAN_POINT('',(-9.18485099360515E-15,-300.,-75.0000000000001));
#5398=CARTESIAN_POINT('Origin',(0.,-300.,-2.77555756156289E-14));
#5399=CARTESIAN_POINT('',(-3.00038465791101E-15,-300.,-24.5));
#5400=CARTESIAN_POINT('Origin',(0.,-300.,-2.77555756156289E-14));
#5401=CARTESIAN_POINT('',(-3.00038465791101E-15,-300.,-24.5));
#5402=CARTESIAN_POINT('Origin',(0.,-300.,-2.77555756156289E-14));
#5403=CARTESIAN_POINT('',(-3.00038465791101E-15,300.,-24.5));
#5404=CARTESIAN_POINT('',(-3.00038465791101E-15,-300.,-24.5));
#5405=CARTESIAN_POINT('Origin',(0.,300.,-2.77555756156289E-14));
#5406=CARTESIAN_POINT('Origin',(0.,-415.,0.));
#5407=CARTESIAN_POINT('Origin',(0.,-300.,0.));
#5408=CARTESIAN_POINT('Origin',(0.,300.,0.));
#5409=CARTESIAN_POINT('Origin',(0.,415.,0.));
#5410=CARTESIAN_POINT('',(0.,0.,0.));
#5411=CARTESIAN_POINT('Origin',(4.99999999999999,0.,0.));
#5412=CARTESIAN_POINT('',(7.34259871723693,0.,0.));
#5413=CARTESIAN_POINT('',(4.99999999999999,-3.00462919747432E-15,-4.0575));
#5414=CARTESIAN_POINT('',(4.99999999999999,-4.96900438754039E-16,-4.0575));
#5415=CARTESIAN_POINT('',(5.,-3.51389807585536,-2.02875));
#5416=CARTESIAN_POINT('Origin',(4.99999999999999,0.,0.));
#5417=CARTESIAN_POINT('',(5.,-3.51389807585536,2.02875));
#5418=CARTESIAN_POINT('Origin',(4.99999999999999,0.,0.));
#5419=CARTESIAN_POINT('',(5.,4.50694379621148E-15,4.0575));
#5420=CARTESIAN_POINT('Origin',(4.99999999999999,0.,0.));
#5421=CARTESIAN_POINT('',(5.,3.51389807585536,2.02875));
#5422=CARTESIAN_POINT('Origin',(4.99999999999999,0.,0.));
#5423=CARTESIAN_POINT('',(5.,3.51389807585536,-2.02875000000001));
#5424=CARTESIAN_POINT('Origin',(4.99999999999999,0.,0.));
#5425=CARTESIAN_POINT('Origin',(4.99999999999999,0.,0.));
#5426=CARTESIAN_POINT('Origin',(10.4,0.,0.));
#5427=CARTESIAN_POINT('',(10.4,6.12323399573681E-16,-5.00000000000003));
#5428=CARTESIAN_POINT('',(10.4,-6.12323399573681E-16,5.00000000000003));
#5429=CARTESIAN_POINT('Origin',(10.4,0.,0.));
#5430=CARTESIAN_POINT('Origin',(10.4,0.,0.));
#5431=CARTESIAN_POINT('',(9.99999999999999,-6.61309271539575E-16,5.40000000000003));
#5432=CARTESIAN_POINT('Origin',(10.4,-6.61309271539575E-16,5.40000000000003));
#5433=CARTESIAN_POINT('Origin',(9.99999999999999,0.,0.));
#5434=CARTESIAN_POINT('Origin',(0.,0.,0.));
#5435=CARTESIAN_POINT('',(1.,9.79717439317883E-16,-8.));
#5436=CARTESIAN_POINT('',(1.,-9.79717439317883E-16,8.));
#5437=CARTESIAN_POINT('Origin',(1.,0.,0.));
#5438=CARTESIAN_POINT('',(-2.69313897121051E-16,-8.57252759403147E-16,7.));
#5439=CARTESIAN_POINT('',(0.,-8.57252759403147E-16,7.));
#5440=CARTESIAN_POINT('Origin',(0.,0.,0.));
#5441=CARTESIAN_POINT('Origin',(1.,0.,0.));
#5442=CARTESIAN_POINT('Origin',(-31.75,0.,0.));
#5443=CARTESIAN_POINT('',(10.,-9.79717439317883E-16,-8.));
#5444=CARTESIAN_POINT('',(-31.75,-9.79717439317883E-16,-8.));
#5445=CARTESIAN_POINT('Origin',(10.,0.,0.));
#5446=CARTESIAN_POINT('Origin',(-31.75,0.,0.));
#5447=CARTESIAN_POINT('',(139.172,-6.12323399573681E-16,-5.00000000000003));
#5448=CARTESIAN_POINT('',(-31.75,-6.12323399573681E-16,-5.00000000000003));
#5449=CARTESIAN_POINT('Origin',(139.172,0.,0.));
#5450=CARTESIAN_POINT('Origin',(140.,0.,0.));
#5451=CARTESIAN_POINT('',(140.,-5.10922644604276E-16,-4.172));
#5452=CARTESIAN_POINT('',(140.,-5.10922644604276E-16,-4.172));
#5453=CARTESIAN_POINT('Origin',(140.,0.,0.));
#5454=CARTESIAN_POINT('Origin',(2.72783148596379E-17,0.,0.));
#5455=CARTESIAN_POINT('',(0.,4.68519743447381,-5.63785129692462E-15));
#5456=CARTESIAN_POINT('',(0.,2.34259871723691,4.0575));
#5457=CARTESIAN_POINT('',(0.,4.68519743447381,-5.63785129692462E-15));
#5458=CARTESIAN_POINT('',(0.,-2.3425987172369,4.0575));
#5459=CARTESIAN_POINT('',(0.,-2.3425987172369,4.0575));
#5460=CARTESIAN_POINT('',(0.,-4.68519743447381,5.63785129692462E-15));
#5461=CARTESIAN_POINT('',(0.,-2.3425987172369,4.0575));
#5462=CARTESIAN_POINT('',(0.,-2.34259871723691,-4.0575));
#5463=CARTESIAN_POINT('',(0.,-4.68519743447381,5.63785129692462E-15));
#5464=CARTESIAN_POINT('',(0.,2.3425987172369,-4.0575));
#5465=CARTESIAN_POINT('',(0.,2.3425987172369,-4.0575));
#5466=CARTESIAN_POINT('',(0.,4.68519743447381,-5.63785129692462E-15));
#5467=CARTESIAN_POINT('Origin',(140.,4.172,0.));
#5468=CARTESIAN_POINT('Origin',(9.99999999999999,8.,0.));
#5469=CARTESIAN_POINT('Origin',(5.,4.68519743447381,-5.63785129692462E-15));
#5470=CARTESIAN_POINT('',(5.,4.68519743447381,-5.63785129692462E-15));
#5471=CARTESIAN_POINT('',(5.,4.68519743447381,-5.63785129692462E-15));
#5472=CARTESIAN_POINT('',(5.,4.68519743447381,-5.63785129692462E-15));
#5473=CARTESIAN_POINT('',(5.,2.34259871723691,4.0575));
#5474=CARTESIAN_POINT('',(5.,4.68519743447381,-5.63785129692462E-15));
#5475=CARTESIAN_POINT('',(5.,2.34259871723691,4.0575));
#5476=CARTESIAN_POINT('Origin',(5.,-2.3425987172369,4.0575));
#5477=CARTESIAN_POINT('',(5.,-2.3425987172369,4.0575));
#5478=CARTESIAN_POINT('',(5.,-2.3425987172369,4.0575));
#5479=CARTESIAN_POINT('',(5.,-2.3425987172369,4.0575));
#5480=CARTESIAN_POINT('',(5.,-2.3425987172369,4.0575));
#5481=CARTESIAN_POINT('Origin',(5.,-2.3425987172369,4.0575));
#5482=CARTESIAN_POINT('',(5.,-2.3425987172369,4.0575));
#5483=CARTESIAN_POINT('',(5.,-4.68519743447381,5.63785129692462E-15));
#5484=CARTESIAN_POINT('',(5.,-2.3425987172369,4.0575));
#5485=CARTESIAN_POINT('',(5.,-4.68519743447381,5.63785129692462E-15));
#5486=CARTESIAN_POINT('Origin',(5.,-4.68519743447381,5.63785129692462E-15));
#5487=CARTESIAN_POINT('',(5.,-4.68519743447381,5.63785129692462E-15));
#5488=CARTESIAN_POINT('',(5.,-2.34259871723691,-4.0575));
#5489=CARTESIAN_POINT('',(5.,-4.68519743447381,5.63785129692462E-15));
#5490=CARTESIAN_POINT('',(5.,-2.34259871723691,-4.0575));
#5491=CARTESIAN_POINT('Origin',(5.,2.3425987172369,-4.0575));
#5492=CARTESIAN_POINT('',(5.,2.3425987172369,-4.0575));
#5493=CARTESIAN_POINT('',(5.,2.3425987172369,-4.0575));
#5494=CARTESIAN_POINT('',(5.,2.3425987172369,-4.0575));
#5495=CARTESIAN_POINT('',(5.,2.3425987172369,-4.0575));
#5496=CARTESIAN_POINT('Origin',(5.,4.68519743447381,-5.63785129692462E-15));
#5497=CARTESIAN_POINT('',(5.,4.68519743447381,-5.63785129692462E-15));
#5498=CARTESIAN_POINT('',(5.,4.68519743447381,-5.63785129692462E-15));
#5499=CARTESIAN_POINT('Origin',(5.,7.02779615171071,-4.05750000000001));
#5500=CARTESIAN_POINT('Origin',(5.,7.02779615171071,-4.05750000000001));
#5501=CARTESIAN_POINT('Origin',(5.,7.02779615171071,-4.05750000000001));
#5502=CARTESIAN_POINT('Origin',(5.,7.02779615171071,-4.05750000000001));
#5503=CARTESIAN_POINT('Origin',(5.,7.02779615171071,-4.05750000000001));
#5504=CARTESIAN_POINT('Origin',(5.,7.02779615171071,-4.05750000000001));
#5505=CARTESIAN_POINT('',(0.,0.,0.));
#5506=CARTESIAN_POINT('Origin',(-34.9249999999999,0.,0.));
#5507=CARTESIAN_POINT('',(-2.3,-1.22464679914735E-15,-10.));
#5508=CARTESIAN_POINT('Origin',(-2.3,0.,0.));
#5509=CARTESIAN_POINT('',(0.,-1.22464679914735E-15,-10.));
#5510=CARTESIAN_POINT('',(-34.9249999999999,-1.22464679914735E-15,-10.));
#5511=CARTESIAN_POINT('Origin',(0.,0.,0.));
#5512=CARTESIAN_POINT('Origin',(-34.9249999999999,0.,0.));
#5513=CARTESIAN_POINT('',(0.,-6.80903620325928E-16,-5.56));
#5514=CARTESIAN_POINT('Origin',(0.,0.,0.));
#5515=CARTESIAN_POINT('',(-2.3,-6.80903620325928E-16,-5.56));
#5516=CARTESIAN_POINT('',(-34.9249999999999,-6.80903620325928E-16,-5.56));
#5517=CARTESIAN_POINT('Origin',(-2.3,0.,0.));
#5518=CARTESIAN_POINT('Origin',(0.,5.56,0.));
#5519=CARTESIAN_POINT('Origin',(-2.3,10.,0.));
#5520=CARTESIAN_POINT('',(0.,0.,0.));
#5521=CARTESIAN_POINT('Origin',(4.00000000000001,0.,0.));
#5522=CARTESIAN_POINT('',(5.75947494535541,0.,0.));
#5523=CARTESIAN_POINT('',(4.,-4.50694379621148E-15,-3.0475));
#5524=CARTESIAN_POINT('',(4.00000000000001,-3.73211112040156E-16,-3.0475));
#5525=CARTESIAN_POINT('',(4.,-2.63921241803308,-1.52375));
#5526=CARTESIAN_POINT('Origin',(4.00000000000001,0.,0.));
#5527=CARTESIAN_POINT('',(4.,-2.63921241803307,1.52375));
#5528=CARTESIAN_POINT('Origin',(4.00000000000001,0.,0.));
#5529=CARTESIAN_POINT('',(4.,2.62905054779003E-15,3.0475));
#5530=CARTESIAN_POINT('Origin',(4.00000000000001,0.,0.));
#5531=CARTESIAN_POINT('',(4.00000000000001,2.63921241803308,1.52375));
#5532=CARTESIAN_POINT('Origin',(4.00000000000001,0.,0.));
#5533=CARTESIAN_POINT('',(4.,2.63921241803308,-1.52375));
#5534=CARTESIAN_POINT('Origin',(4.00000000000001,0.,0.));
#5535=CARTESIAN_POINT('Origin',(4.00000000000001,0.,0.));
#5536=CARTESIAN_POINT('Origin',(8.4,0.,0.));
#5537=CARTESIAN_POINT('',(8.4,4.89858719658945E-16,-4.00000000000003));
#5538=CARTESIAN_POINT('',(8.4,-4.89858719658945E-16,4.00000000000003));
#5539=CARTESIAN_POINT('Origin',(8.4,0.,0.));
#5540=CARTESIAN_POINT('Origin',(8.4,0.,0.));
#5541=CARTESIAN_POINT('',(8.,-5.38844591624839E-16,4.40000000000003));
#5542=CARTESIAN_POINT('Origin',(8.4,-5.38844591624839E-16,4.40000000000003));
#5543=CARTESIAN_POINT('Origin',(8.,0.,0.));
#5544=CARTESIAN_POINT('Origin',(33.,0.,0.));
#5545=CARTESIAN_POINT('',(32.3095000000001,-4.89858719658949E-16,-4.00000000000006));
#5546=CARTESIAN_POINT('Origin',(32.3095000000001,0.,0.));
#5547=CARTESIAN_POINT('',(33.,-4.05296858177817E-16,-3.3095));
#5548=CARTESIAN_POINT('',(33.,-4.05296858177817E-16,-3.3095));
#5549=CARTESIAN_POINT('Origin',(33.,0.,0.));
#5550=CARTESIAN_POINT('Origin',(-31.75,0.,0.));
#5551=CARTESIAN_POINT('',(-31.75,-4.89858719658945E-16,-4.00000000000003));
#5552=CARTESIAN_POINT('Origin',(-31.75,0.,0.));
#5553=CARTESIAN_POINT('',(0.800000000000002,7.9602041944578E-16,6.5));
#5554=CARTESIAN_POINT('',(0.800000000000001,-7.9602041944578E-16,-6.5));
#5555=CARTESIAN_POINT('Origin',(0.800000000000002,0.,0.));
#5556=CARTESIAN_POINT('Origin',(0.800000000000002,0.,0.));
#5557=CARTESIAN_POINT('',(8.00000000000001,-7.9602041944578E-16,-6.5));
#5558=CARTESIAN_POINT('',(-31.75,-7.9602041944578E-16,-6.5));
#5559=CARTESIAN_POINT('Origin',(8.00000000000001,0.,0.));
#5560=CARTESIAN_POINT('Origin',(0.,0.,0.));
#5561=CARTESIAN_POINT('',(-2.19298459084284E-16,-6.98048675513992E-16,5.7));
#5562=CARTESIAN_POINT('',(0.,-6.98048675513992E-16,5.7));
#5563=CARTESIAN_POINT('Origin',(0.,0.,0.));
#5564=CARTESIAN_POINT('Origin',(-3.19315087200652E-17,0.,0.));
#5565=CARTESIAN_POINT('',(0.,3.51894989071077,-3.46944695195361E-15));
#5566=CARTESIAN_POINT('',(0.,1.75947494535539,3.0475));
#5567=CARTESIAN_POINT('',(0.,3.51894989071077,-3.46944695195361E-15));
#5568=CARTESIAN_POINT('',(0.,-1.75947494535538,3.0475));
#5569=CARTESIAN_POINT('',(0.,-1.75947494535538,3.0475));
#5570=CARTESIAN_POINT('',(0.,-3.51894989071077,5.20417042793042E-15));
#5571=CARTESIAN_POINT('',(0.,-1.75947494535538,3.0475));
#5572=CARTESIAN_POINT('',(0.,-1.75947494535539,-3.0475));
#5573=CARTESIAN_POINT('',(0.,-3.51894989071077,5.20417042793042E-15));
#5574=CARTESIAN_POINT('',(0.,1.75947494535538,-3.0475));
#5575=CARTESIAN_POINT('',(0.,1.75947494535538,-3.0475));
#5576=CARTESIAN_POINT('',(0.,3.51894989071077,-3.46944695195361E-15));
#5577=CARTESIAN_POINT('Origin',(8.,6.5,0.));
#5578=CARTESIAN_POINT('Origin',(33.,3.3095,0.));
#5579=CARTESIAN_POINT('Origin',(4.,3.51894989071077,-3.46944695195361E-15));
#5580=CARTESIAN_POINT('',(4.,3.51894989071077,-3.46944695195361E-15));
#5581=CARTESIAN_POINT('',(4.,3.51894989071077,-3.46944695195361E-15));
#5582=CARTESIAN_POINT('',(4.,3.51894989071077,-3.46944695195361E-15));
#5583=CARTESIAN_POINT('',(4.,1.75947494535539,3.0475));
#5584=CARTESIAN_POINT('',(4.,3.51894989071077,-3.46944695195361E-15));
#5585=CARTESIAN_POINT('',(4.,1.75947494535539,3.0475));
#5586=CARTESIAN_POINT('Origin',(4.,-1.75947494535538,3.0475));
#5587=CARTESIAN_POINT('',(4.,-1.75947494535538,3.0475));
#5588=CARTESIAN_POINT('',(4.,-1.75947494535538,3.0475));
#5589=CARTESIAN_POINT('',(4.,-1.75947494535538,3.0475));
#5590=CARTESIAN_POINT('',(4.,-1.75947494535538,3.0475));
#5591=CARTESIAN_POINT('Origin',(4.,-1.75947494535538,3.0475));
#5592=CARTESIAN_POINT('',(4.,-1.75947494535538,3.0475));
#5593=CARTESIAN_POINT('',(4.,-3.51894989071077,5.20417042793042E-15));
#5594=CARTESIAN_POINT('',(4.,-1.75947494535538,3.0475));
#5595=CARTESIAN_POINT('',(4.,-3.51894989071077,5.20417042793042E-15));
#5596=CARTESIAN_POINT('Origin',(4.,-3.51894989071077,5.20417042793042E-15));
#5597=CARTESIAN_POINT('',(4.,-3.51894989071077,5.20417042793042E-15));
#5598=CARTESIAN_POINT('',(4.,-1.75947494535539,-3.0475));
#5599=CARTESIAN_POINT('',(4.,-3.51894989071077,5.20417042793042E-15));
#5600=CARTESIAN_POINT('',(4.,-1.75947494535539,-3.0475));
#5601=CARTESIAN_POINT('Origin',(4.,1.75947494535538,-3.0475));
#5602=CARTESIAN_POINT('',(4.,1.75947494535538,-3.0475));
#5603=CARTESIAN_POINT('',(4.,1.75947494535538,-3.0475));
#5604=CARTESIAN_POINT('',(4.,1.75947494535538,-3.0475));
#5605=CARTESIAN_POINT('',(4.,1.75947494535538,-3.0475));
#5606=CARTESIAN_POINT('Origin',(4.,3.51894989071077,-3.46944695195361E-15));
#5607=CARTESIAN_POINT('',(4.,3.51894989071077,-3.46944695195361E-15));
#5608=CARTESIAN_POINT('',(4.,3.51894989071077,-3.46944695195361E-15));
#5609=CARTESIAN_POINT('Origin',(4.,1.75947494535539,3.0475));
#5610=CARTESIAN_POINT('Origin',(4.,1.75947494535539,3.0475));
#5611=CARTESIAN_POINT('Origin',(4.,1.75947494535539,3.0475));
#5612=CARTESIAN_POINT('Origin',(4.,1.75947494535539,3.0475));
#5613=CARTESIAN_POINT('Origin',(4.,1.75947494535539,3.0475));
#5614=CARTESIAN_POINT('Origin',(4.,1.75947494535539,3.0475));
#5615=CARTESIAN_POINT('',(-350.,0.,0.));
#5616=CARTESIAN_POINT('',(3.02021568005662E-16,-425.,-8.67361737988404E-16));
#5617=CARTESIAN_POINT('',(0.,0.,0.));
#5618=CARTESIAN_POINT('',(-335.,49.9999999999999,50.0000000000001));
#5619=CARTESIAN_POINT('',(-455.,1.76941794549634E-13,60.));
#5620=CARTESIAN_POINT('',(-190.,0.,460.));
#5621=CARTESIAN_POINT('',(-350.,-30.,70.));
#5622=CARTESIAN_POINT('',(-350.,30.,-50.));
#5623=CARTESIAN_POINT('',(-350.,30.,-60.7));
#5624=CARTESIAN_POINT('',(-350.,-30.,-60.7));
#5625=CARTESIAN_POINT('',(-487.5,2.04697370165263E-13,78.4));
#5626=CARTESIAN_POINT('',(350.,-1.19455362485379E-13,-4.16333634234434E-14));
#5627=CARTESIAN_POINT('',(-4.85326548186048E-16,425.,5.03069808033274E-14));
#5628=CARTESIAN_POINT('',(-350.,30.,70.));
#5629=CARTESIAN_POINT('',(-350.,-30.,-50.));
#5630=CARTESIAN_POINT('',(-455.,-32.4999999999998,78.3999999999999));
#5631=CARTESIAN_POINT('',(-455.,32.5000000000002,78.4));
#5632=CARTESIAN_POINT('',(-422.5,8.32667268468867E-14,78.4));
#5633=UNCERTAINTY_MEASURE_WITH_UNIT(LENGTH_MEASURE(0.01),#5659,
'DISTANCE_ACCURACY_VALUE',
'Maximum model space distance between geometric entities at asserted c
onnectivities');
#5634=UNCERTAINTY_MEASURE_WITH_UNIT(LENGTH_MEASURE(0.01),#5659,
'DISTANCE_ACCURACY_VALUE',
'Maximum model space distance between geometric entities at asserted c
onnectivities');
#5635=UNCERTAINTY_MEASURE_WITH_UNIT(LENGTH_MEASURE(0.01),#5659,
'DISTANCE_ACCURACY_VALUE',
'Maximum model space distance between geometric entities at asserted c
onnectivities');
#5636=UNCERTAINTY_MEASURE_WITH_UNIT(LENGTH_MEASURE(0.01),#5659,
'DISTANCE_ACCURACY_VALUE',
'Maximum model space distance between geometric entities at asserted c
onnectivities');
#5637=UNCERTAINTY_MEASURE_WITH_UNIT(LENGTH_MEASURE(0.01),#5659,
'DISTANCE_ACCURACY_VALUE',
'Maximum model space distance between geometric entities at asserted c
onnectivities');
#5638=UNCERTAINTY_MEASURE_WITH_UNIT(LENGTH_MEASURE(0.01),#5659,
'DISTANCE_ACCURACY_VALUE',
'Maximum model space distance between geometric entities at asserted c
onnectivities');
#5639=UNCERTAINTY_MEASURE_WITH_UNIT(LENGTH_MEASURE(0.01),#5659,
'DISTANCE_ACCURACY_VALUE',
'Maximum model space distance between geometric entities at asserted c
onnectivities');
#5640=UNCERTAINTY_MEASURE_WITH_UNIT(LENGTH_MEASURE(0.01),#5659,
'DISTANCE_ACCURACY_VALUE',
'Maximum model space distance between geometric entities at asserted c
onnectivities');
#5641=UNCERTAINTY_MEASURE_WITH_UNIT(LENGTH_MEASURE(0.01),#5659,
'DISTANCE_ACCURACY_VALUE',
'Maximum model space distance between geometric entities at asserted c
onnectivities');
#5642=UNCERTAINTY_MEASURE_WITH_UNIT(LENGTH_MEASURE(0.01),#5659,
'DISTANCE_ACCURACY_VALUE',
'Maximum model space distance between geometric entities at asserted c
onnectivities');
#5643=UNCERTAINTY_MEASURE_WITH_UNIT(LENGTH_MEASURE(0.01),#5659,
'DISTANCE_ACCURACY_VALUE',
'Maximum model space distance between geometric entities at asserted c
onnectivities');
#5644=UNCERTAINTY_MEASURE_WITH_UNIT(LENGTH_MEASURE(0.01),#5659,
'DISTANCE_ACCURACY_VALUE',
'Maximum model space distance between geometric entities at asserted c
onnectivities');
#5645=UNCERTAINTY_MEASURE_WITH_UNIT(LENGTH_MEASURE(0.01),#5659,
'DISTANCE_ACCURACY_VALUE',
'Maximum model space distance between geometric entities at asserted c
onnectivities');
#5646=(
GEOMETRIC_REPRESENTATION_CONTEXT(3)
GLOBAL_UNCERTAINTY_ASSIGNED_CONTEXT((#5633))
GLOBAL_UNIT_ASSIGNED_CONTEXT((#5659,#5661,#5662))
REPRESENTATION_CONTEXT('','3D')
);
#5647=(
GEOMETRIC_REPRESENTATION_CONTEXT(3)
GLOBAL_UNCERTAINTY_ASSIGNED_CONTEXT((#5634))
GLOBAL_UNIT_ASSIGNED_CONTEXT((#5659,#5661,#5662))
REPRESENTATION_CONTEXT('','3D')
);
#5648=(
GEOMETRIC_REPRESENTATION_CONTEXT(3)
GLOBAL_UNCERTAINTY_ASSIGNED_CONTEXT((#5635))
GLOBAL_UNIT_ASSIGNED_CONTEXT((#5659,#5661,#5662))
REPRESENTATION_CONTEXT('','3D')
);
#5649=(
GEOMETRIC_REPRESENTATION_CONTEXT(3)
GLOBAL_UNCERTAINTY_ASSIGNED_CONTEXT((#5636))
GLOBAL_UNIT_ASSIGNED_CONTEXT((#5659,#5661,#5662))
REPRESENTATION_CONTEXT('','3D')
);
#5650=(
GEOMETRIC_REPRESENTATION_CONTEXT(3)
GLOBAL_UNCERTAINTY_ASSIGNED_CONTEXT((#5637))
GLOBAL_UNIT_ASSIGNED_CONTEXT((#5659,#5661,#5662))
REPRESENTATION_CONTEXT('','3D')
);
#5651=(
GEOMETRIC_REPRESENTATION_CONTEXT(3)
GLOBAL_UNCERTAINTY_ASSIGNED_CONTEXT((#5638))
GLOBAL_UNIT_ASSIGNED_CONTEXT((#5659,#5661,#5662))
REPRESENTATION_CONTEXT('','3D')
);
#5652=(
GEOMETRIC_REPRESENTATION_CONTEXT(3)
GLOBAL_UNCERTAINTY_ASSIGNED_CONTEXT((#5639))
GLOBAL_UNIT_ASSIGNED_CONTEXT((#5659,#5661,#5662))
REPRESENTATION_CONTEXT('','3D')
);
#5653=(
GEOMETRIC_REPRESENTATION_CONTEXT(3)
GLOBAL_UNCERTAINTY_ASSIGNED_CONTEXT((#5640))
GLOBAL_UNIT_ASSIGNED_CONTEXT((#5659,#5661,#5662))
REPRESENTATION_CONTEXT('','3D')
);
#5654=(
GEOMETRIC_REPRESENTATION_CONTEXT(3)
GLOBAL_UNCERTAINTY_ASSIGNED_CONTEXT((#5641))
GLOBAL_UNIT_ASSIGNED_CONTEXT((#5659,#5661,#5662))
REPRESENTATION_CONTEXT('','3D')
);
#5655=(
GEOMETRIC_REPRESENTATION_CONTEXT(3)
GLOBAL_UNCERTAINTY_ASSIGNED_CONTEXT((#5642))
GLOBAL_UNIT_ASSIGNED_CONTEXT((#5659,#5661,#5662))
REPRESENTATION_CONTEXT('','3D')
);
#5656=(
GEOMETRIC_REPRESENTATION_CONTEXT(3)
GLOBAL_UNCERTAINTY_ASSIGNED_CONTEXT((#5643))
GLOBAL_UNIT_ASSIGNED_CONTEXT((#5659,#5661,#5662))
REPRESENTATION_CONTEXT('','3D')
);
#5657=(
GEOMETRIC_REPRESENTATION_CONTEXT(3)
GLOBAL_UNCERTAINTY_ASSIGNED_CONTEXT((#5644))
GLOBAL_UNIT_ASSIGNED_CONTEXT((#5659,#5661,#5662))
REPRESENTATION_CONTEXT('','3D')
);
#5658=(
GEOMETRIC_REPRESENTATION_CONTEXT(3)
GLOBAL_UNCERTAINTY_ASSIGNED_CONTEXT((#5645))
GLOBAL_UNIT_ASSIGNED_CONTEXT((#5659,#5661,#5662))
REPRESENTATION_CONTEXT('','3D')
);
#5659=(
LENGTH_UNIT()
NAMED_UNIT(*)
SI_UNIT(.MILLI.,.METRE.)
);
#5660=(
LENGTH_UNIT()
NAMED_UNIT(*)
SI_UNIT($,.METRE.)
);
#5661=(
NAMED_UNIT(*)
PLANE_ANGLE_UNIT()
SI_UNIT($,.RADIAN.)
);
#5662=(
NAMED_UNIT(*)
SI_UNIT($,.STERADIAN.)
SOLID_ANGLE_UNIT()
);
#5663=SHAPE_DEFINITION_REPRESENTATION(#5675,#5705);
#5664=SHAPE_DEFINITION_REPRESENTATION(#5676,#5706);
#5665=SHAPE_DEFINITION_REPRESENTATION(#5677,#5707);
#5666=SHAPE_DEFINITION_REPRESENTATION(#5678,#5708);
#5667=SHAPE_DEFINITION_REPRESENTATION(#5679,#5709);
#5668=SHAPE_DEFINITION_REPRESENTATION(#5680,#5710);
#5669=SHAPE_DEFINITION_REPRESENTATION(#5681,#5711);
#5670=SHAPE_DEFINITION_REPRESENTATION(#5682,#5712);
#5671=SHAPE_DEFINITION_REPRESENTATION(#5683,#5713);
#5672=SHAPE_DEFINITION_REPRESENTATION(#5684,#5714);
#5673=SHAPE_DEFINITION_REPRESENTATION(#5685,#5715);
#5674=SHAPE_DEFINITION_REPRESENTATION(#5686,#5716);
#5675=PRODUCT_DEFINITION_SHAPE('',$,#5718);
#5676=PRODUCT_DEFINITION_SHAPE('',$,#5719);
#5677=PRODUCT_DEFINITION_SHAPE('',$,#5720);
#5678=PRODUCT_DEFINITION_SHAPE('',$,#5721);
#5679=PRODUCT_DEFINITION_SHAPE('',$,#5722);
#5680=PRODUCT_DEFINITION_SHAPE('',$,#5723);
#5681=PRODUCT_DEFINITION_SHAPE('',$,#5724);
#5682=PRODUCT_DEFINITION_SHAPE('',$,#5725);
#5683=PRODUCT_DEFINITION_SHAPE('',$,#5726);
#5684=PRODUCT_DEFINITION_SHAPE('',$,#5727);
#5685=PRODUCT_DEFINITION_SHAPE('',$,#5728);
#5686=PRODUCT_DEFINITION_SHAPE('',$,#5729);
#5687=PRODUCT_DEFINITION_SHAPE($,$,#65);
#5688=PRODUCT_DEFINITION_SHAPE($,$,#66);
#5689=PRODUCT_DEFINITION_SHAPE($,$,#67);
#5690=PRODUCT_DEFINITION_SHAPE($,$,#68);
#5691=PRODUCT_DEFINITION_SHAPE($,$,#69);
#5692=PRODUCT_DEFINITION_SHAPE($,$,#70);
#5693=PRODUCT_DEFINITION_SHAPE($,$,#71);
#5694=PRODUCT_DEFINITION_SHAPE($,$,#72);
#5695=PRODUCT_DEFINITION_SHAPE($,$,#73);
#5696=PRODUCT_DEFINITION_SHAPE($,$,#74);
#5697=PRODUCT_DEFINITION_SHAPE($,$,#75);
#5698=PRODUCT_DEFINITION_SHAPE($,$,#76);
#5699=PRODUCT_DEFINITION_SHAPE($,$,#77);
#5700=PRODUCT_DEFINITION_SHAPE($,$,#78);
#5701=PRODUCT_DEFINITION_SHAPE($,$,#79);
#5702=PRODUCT_DEFINITION_SHAPE($,$,#80);
#5703=PRODUCT_DEFINITION_SHAPE($,$,#81);
#5704=PRODUCT_DEFINITION_SHAPE($,$,#82);
#5705=SHAPE_REPRESENTATION('',(#3193,#3541,#3542,#3543,#3544,#3545,#3546,
#3547,#3548,#3549,#3550,#3551,#3552,#3553,#3554,#3555,#3556,#3557,#3558),
#5646);
#5706=SHAPE_REPRESENTATION('',(#3194),#5647);
#5707=SHAPE_REPRESENTATION('',(#3213),#5648);
#5708=SHAPE_REPRESENTATION('',(#3240),#5649);
#5709=SHAPE_REPRESENTATION('',(#3278),#5650);
#5710=SHAPE_REPRESENTATION('',(#3325),#5651);
#5711=SHAPE_REPRESENTATION('',(#3361),#5652);
#5712=SHAPE_REPRESENTATION('',(#3397),#5653);
#5713=SHAPE_REPRESENTATION('',(#3432),#5654);
#5714=SHAPE_REPRESENTATION('',(#3456),#5655);
#5715=SHAPE_REPRESENTATION('',(#3494),#5656);
#5716=SHAPE_REPRESENTATION('',(#3503),#5657);
#5717=PRODUCT_DEFINITION_CONTEXT('part definition',#5755,'design');
#5718=PRODUCT_DEFINITION('MAT-030','MAT-030',#5730,#5717);
#5719=PRODUCT_DEFINITION('Conveyor Belt','Conveyor Belt',#5731,#5717);
#5720=PRODUCT_DEFINITION('Column Mount Bracket','Column Mount Bracket',
#5732,#5717);
#5721=PRODUCT_DEFINITION('Camera Arm','Camera Arm',#5733,#5717);
#5722=PRODUCT_DEFINITION('Camera','Camera',#5734,#5717);
#5723=PRODUCT_DEFINITION('Hex Nut M10 x 1.5 (2)',
'Hex Nut M10 x 1.5 (2)',#5735,#5717);
#5724=PRODUCT_DEFINITION('Hex Nut M10 x 1.5','Hex Nut M10 x 1.5',#5736,
#5717);
#5725=PRODUCT_DEFINITION('Rectangular Tube 100 x 100 x 5',
'Rectangular Tube 100 x 100 x 5',#5737,#5717);
#5726=PRODUCT_DEFINITION('Conveyor Roller','Conveyor Roller',#5738,#5717);
#5727=PRODUCT_DEFINITION('Socket Head Cap Screw M10 x 1.5 x 130',
'Socket Head Cap Screw M10 x 1.5 x 130',#5739,#5717);
#5728=PRODUCT_DEFINITION('Flat Washer M10 Narrow',
'Flat Washer M10 Narrow',#5740,#5717);
#5729=PRODUCT_DEFINITION('Socket Head Cap Screw M8 x 1.25 x 25',
'Socket Head Cap Screw M8 x 1.25 x 25',#5741,#5717);
#5730=PRODUCT_DEFINITION_FORMATION('',$,#5757);
#5731=PRODUCT_DEFINITION_FORMATION('',$,#5758);
#5732=PRODUCT_DEFINITION_FORMATION('',$,#5759);
#5733=PRODUCT_DEFINITION_FORMATION('',$,#5760);
#5734=PRODUCT_DEFINITION_FORMATION('',$,#5761);
#5735=PRODUCT_DEFINITION_FORMATION('',$,#5762);
#5736=PRODUCT_DEFINITION_FORMATION('',$,#5763);
#5737=PRODUCT_DEFINITION_FORMATION('',$,#5764);
#5738=PRODUCT_DEFINITION_FORMATION('',$,#5765);
#5739=PRODUCT_DEFINITION_FORMATION('',$,#5766);
#5740=PRODUCT_DEFINITION_FORMATION('',$,#5767);
#5741=PRODUCT_DEFINITION_FORMATION('',$,#5768);
#5742=PRODUCT_RELATED_PRODUCT_CATEGORY('MAT-030','MAT-030',(#5757));
#5743=PRODUCT_RELATED_PRODUCT_CATEGORY('Conveyor Belt','Conveyor Belt',
(#5758));
#5744=PRODUCT_RELATED_PRODUCT_CATEGORY('Column Mount Bracket',
'Column Mount Bracket',(#5759));
#5745=PRODUCT_RELATED_PRODUCT_CATEGORY('Camera Arm','Camera Arm',(#5760));
#5746=PRODUCT_RELATED_PRODUCT_CATEGORY('Camera','Camera',(#5761));
#5747=PRODUCT_RELATED_PRODUCT_CATEGORY('Hex Nut M10 x 1.5 (2)',
'Hex Nut M10 x 1.5 (2)',(#5762));
#5748=PRODUCT_RELATED_PRODUCT_CATEGORY('Hex Nut M10 x 1.5',
'Hex Nut M10 x 1.5',(#5763));
#5749=PRODUCT_RELATED_PRODUCT_CATEGORY('Rectangular Tube 100 x 100 x 5',
'Rectangular Tube 100 x 100 x 5',(#5764));
#5750=PRODUCT_RELATED_PRODUCT_CATEGORY('Conveyor Roller',
'Conveyor Roller',(#5765));
#5751=PRODUCT_RELATED_PRODUCT_CATEGORY(
'Socket Head Cap Screw M10 x 1.5 x 130',
'Socket Head Cap Screw M10 x 1.5 x 130',(#5766));
#5752=PRODUCT_RELATED_PRODUCT_CATEGORY('Flat Washer M10 Narrow',
'Flat Washer M10 Narrow',(#5767));
#5753=PRODUCT_RELATED_PRODUCT_CATEGORY(
'Socket Head Cap Screw M8 x 1.25 x 25',
'Socket Head Cap Screw M8 x 1.25 x 25',(#5768));
#5754=APPLICATION_PROTOCOL_DEFINITION('international standard',
'automotive_design',2009,#5755);
#5755=APPLICATION_CONTEXT(
'Core Data for Automotive Mechanical Design Process');
#5756=PRODUCT_CONTEXT('part definition',#5755,'mechanical');
#5757=PRODUCT('MAT-030','MAT-030','STEP AP214',(#5756));
#5758=PRODUCT('Conveyor Belt','Conveyor Belt',$,(#5756));
#5759=PRODUCT('Column Mount Bracket','Column Mount Bracket',$,(#5756));
#5760=PRODUCT('Camera Arm','Camera Arm',$,(#5756));
#5761=PRODUCT('Camera','Camera',$,(#5756));
#5762=PRODUCT('Hex Nut M10 x 1.5 (2)','Hex Nut M10 x 1.5 (2)',$,(#5756));
#5763=PRODUCT('Hex Nut M10 x 1.5','Hex Nut M10 x 1.5',$,(#5756));
#5764=PRODUCT('Rectangular Tube 100 x 100 x 5',
'Rectangular Tube 100 x 100 x 5',$,(#5756));
#5765=PRODUCT('Conveyor Roller','Conveyor Roller',$,(#5756));
#5766=PRODUCT('Socket Head Cap Screw M10 x 1.5 x 130',
'Socket Head Cap Screw M10 x 1.5 x 130',$,(#5756));
#5767=PRODUCT('Flat Washer M10 Narrow','Flat Washer M10 Narrow',$,(#5756));
#5768=PRODUCT('Socket Head Cap Screw M8 x 1.25 x 25',
'Socket Head Cap Screw M8 x 1.25 x 25',$,(#5756));
#5769=PRESENTATION_STYLE_ASSIGNMENT((#5774));
#5770=PRESENTATION_STYLE_ASSIGNMENT((#5775));
#5771=PRESENTATION_STYLE_ASSIGNMENT((#5776));
#5772=PRESENTATION_STYLE_ASSIGNMENT((#5777));
#5773=PRESENTATION_STYLE_ASSIGNMENT((#5778));
#5774=SURFACE_STYLE_USAGE(.BOTH.,#5779);
#5775=SURFACE_STYLE_USAGE(.BOTH.,#5780);
#5776=SURFACE_STYLE_USAGE(.BOTH.,#5781);
#5777=SURFACE_STYLE_USAGE(.BOTH.,#5782);
#5778=SURFACE_STYLE_USAGE(.BOTH.,#5783);
#5779=SURFACE_SIDE_STYLE('',(#5784));
#5780=SURFACE_SIDE_STYLE('',(#5785));
#5781=SURFACE_SIDE_STYLE('',(#5786));
#5782=SURFACE_SIDE_STYLE('',(#5787));
#5783=SURFACE_SIDE_STYLE('',(#5788));
#5784=SURFACE_STYLE_FILL_AREA(#5789);
#5785=SURFACE_STYLE_FILL_AREA(#5790);
#5786=SURFACE_STYLE_FILL_AREA(#5791);
#5787=SURFACE_STYLE_FILL_AREA(#5792);
#5788=SURFACE_STYLE_FILL_AREA(#5793);
#5789=FILL_AREA_STYLE('Steel - Satin',(#5794));
#5790=FILL_AREA_STYLE('Opaque(31,36,43)',(#5795));
#5791=FILL_AREA_STYLE('Opaque(20,51,87)',(#5796));
#5792=FILL_AREA_STYLE('Opaque(227,224,212)',(#5797));
#5793=FILL_AREA_STYLE('Opaque(61,176,222)',(#5798));
#5794=FILL_AREA_STYLE_COLOUR('Steel - Satin',#5799);
#5795=FILL_AREA_STYLE_COLOUR('Opaque(31,36,43)',#5800);
#5796=FILL_AREA_STYLE_COLOUR('Opaque(20,51,87)',#5801);
#5797=FILL_AREA_STYLE_COLOUR('Opaque(227,224,212)',#5802);
#5798=FILL_AREA_STYLE_COLOUR('Opaque(61,176,222)',#5803);
#5799=COLOUR_RGB('Steel - Satin',0.627450980392157,0.627450980392157,0.627450980392157);
#5800=COLOUR_RGB('Opaque(31,36,43)',0.12156862745098,0.141176470588235,
0.168627450980392);
#5801=COLOUR_RGB('Opaque(20,51,87)',0.0784313725490196,0.2,0.341176470588235);
#5802=COLOUR_RGB('Opaque(227,224,212)',0.890196078431372,0.87843137254902,
0.831372549019608);
#5803=COLOUR_RGB('Opaque(61,176,222)',0.23921568627451,0.690196078431373,
0.870588235294118);
ENDSEC;
END-ISO-10303-21;
